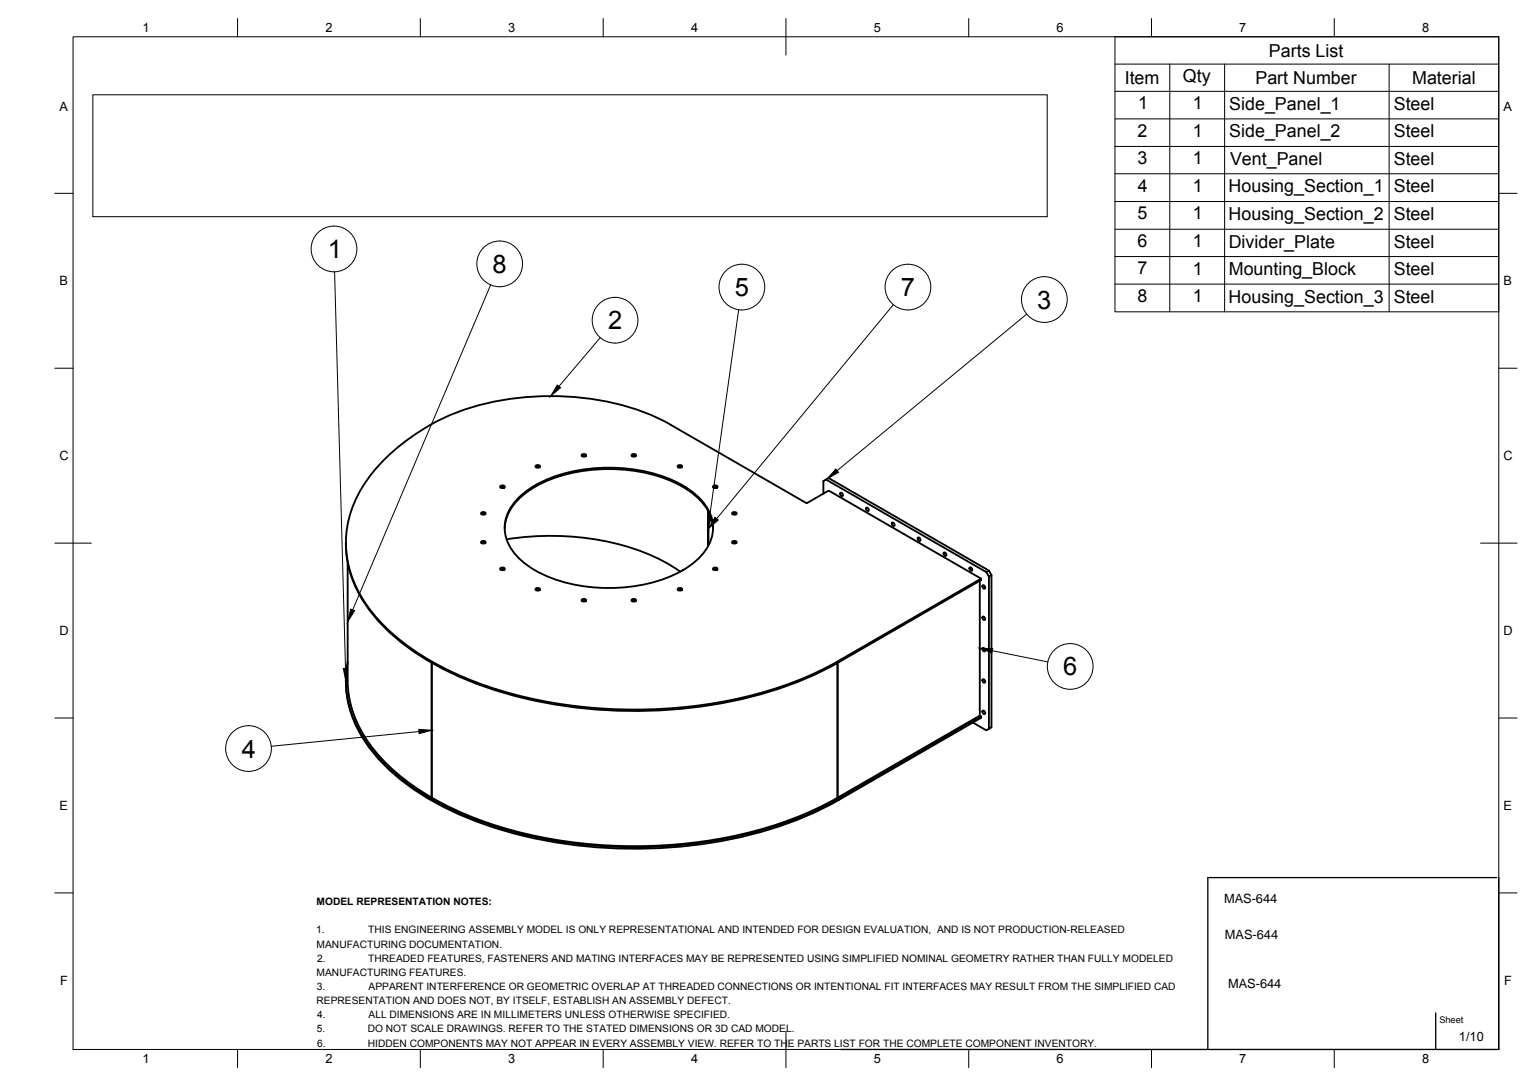
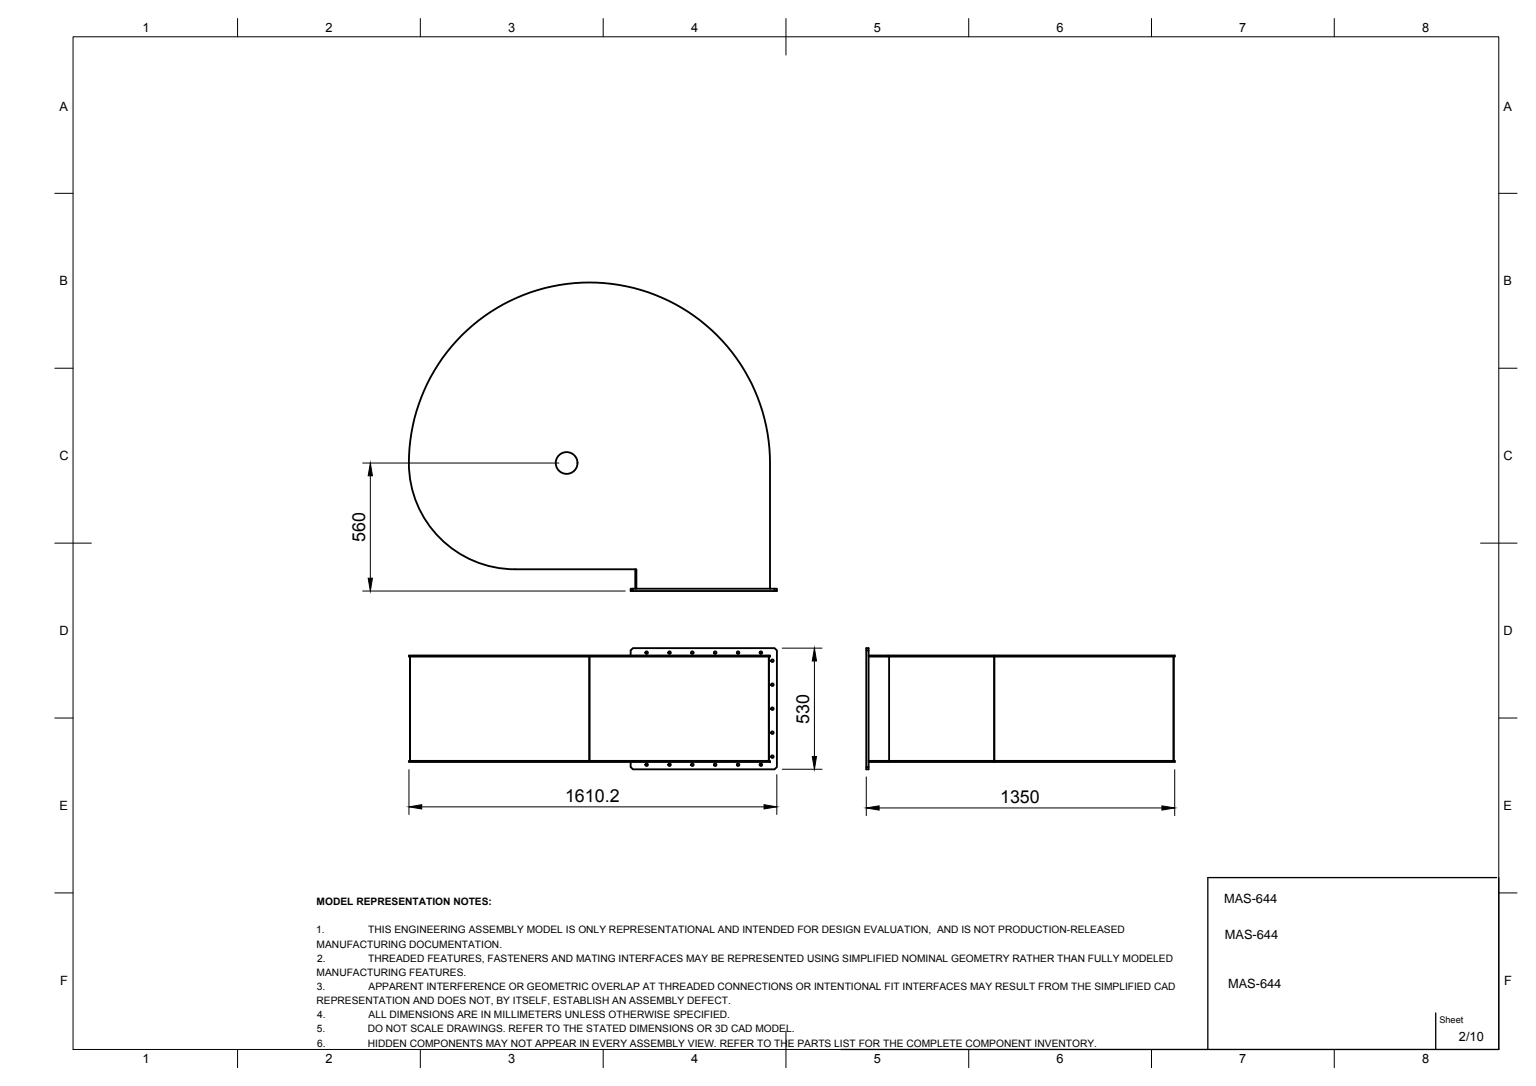
ISO-10303-21;
HEADER;
FILE_DESCRIPTION((''),'2;1');
FILE_NAME('MAS-644','2026-10-09T11:38:21-07:00',(''),(''),'','','');
FILE_SCHEMA (('AUTOMOTIVE_DESIGN { 1 0 10303 214 3 1 1 }'));
ENDSEC;
DATA;
#10 = MECHANICAL_DESIGN_GEOMETRIC_PRESENTATION_REPRESENTATION('',(#59,#60,
#61,#62,#63,#64,#65,#66),#3619) ;
#11 = ITEM_DEFINED_TRANSFORMATION($,$,#2181,#2401) ;
#12 = ITEM_DEFINED_TRANSFORMATION($,$,#2197,#2402) ;
#13 = ITEM_DEFINED_TRANSFORMATION($,$,#2261,#2403) ;
#14 = ITEM_DEFINED_TRANSFORMATION($,$,#2342,#2404) ;
#15 = ITEM_DEFINED_TRANSFORMATION($,$,#2353,#2405) ;
#16 = ITEM_DEFINED_TRANSFORMATION($,$,#2364,#2406) ;
#17 = ITEM_DEFINED_TRANSFORMATION($,$,#2371,#2407) ;
#18 = ITEM_DEFINED_TRANSFORMATION($,$,#2390,#2408) ;
#19 = (
REPRESENTATION_RELATIONSHIP($,$,#3651,#3650)
REPRESENTATION_RELATIONSHIP_WITH_TRANSFORMATION(#11)
SHAPE_REPRESENTATION_RELATIONSHIP()
) ;
#20 = (
REPRESENTATION_RELATIONSHIP($,$,#3652,#3650)
REPRESENTATION_RELATIONSHIP_WITH_TRANSFORMATION(#12)
SHAPE_REPRESENTATION_RELATIONSHIP()
) ;
#21 = (
REPRESENTATION_RELATIONSHIP($,$,#3653,#3650)
REPRESENTATION_RELATIONSHIP_WITH_TRANSFORMATION(#13)
SHAPE_REPRESENTATION_RELATIONSHIP()
) ;
#22 = (
REPRESENTATION_RELATIONSHIP($,$,#3654,#3650)
REPRESENTATION_RELATIONSHIP_WITH_TRANSFORMATION(#14)
SHAPE_REPRESENTATION_RELATIONSHIP()
) ;
#23 = (
REPRESENTATION_RELATIONSHIP($,$,#3655,#3650)
REPRESENTATION_RELATIONSHIP_WITH_TRANSFORMATION(#15)
SHAPE_REPRESENTATION_RELATIONSHIP()
) ;
#24 = (
REPRESENTATION_RELATIONSHIP($,$,#3656,#3650)
REPRESENTATION_RELATIONSHIP_WITH_TRANSFORMATION(#16)
SHAPE_REPRESENTATION_RELATIONSHIP()
) ;
#25 = (
REPRESENTATION_RELATIONSHIP($,$,#3657,#3650)
REPRESENTATION_RELATIONSHIP_WITH_TRANSFORMATION(#17)
SHAPE_REPRESENTATION_RELATIONSHIP()
) ;
#26 = (
REPRESENTATION_RELATIONSHIP($,$,#3658,#3650)
REPRESENTATION_RELATIONSHIP_WITH_TRANSFORMATION(#18)
SHAPE_REPRESENTATION_RELATIONSHIP()
) ;
#27 = CONTEXT_DEPENDENT_SHAPE_REPRESENTATION(#19,#3642) ;
#28 = CONTEXT_DEPENDENT_SHAPE_REPRESENTATION(#20,#3643) ;
#29 = CONTEXT_DEPENDENT_SHAPE_REPRESENTATION(#21,#3644) ;
#30 = CONTEXT_DEPENDENT_SHAPE_REPRESENTATION(#22,#3645) ;
#31 = CONTEXT_DEPENDENT_SHAPE_REPRESENTATION(#23,#3646) ;
#32 = CONTEXT_DEPENDENT_SHAPE_REPRESENTATION(#24,#3647) ;
#33 = CONTEXT_DEPENDENT_SHAPE_REPRESENTATION(#25,#3648) ;
#34 = CONTEXT_DEPENDENT_SHAPE_REPRESENTATION(#26,#3649) ;
#35 = NEXT_ASSEMBLY_USAGE_OCCURRENCE('Side_Panel_1:1','Side_Panel_1:1',
'Side_Panel_1:1',#3660,#3661,'Side_Panel_1:1') ;
#36 = NEXT_ASSEMBLY_USAGE_OCCURRENCE('Side_Panel_2:1','Side_Panel_2:1',
'Side_Panel_2:1',#3660,#3662,'Side_Panel_2:1') ;
#37 = NEXT_ASSEMBLY_USAGE_OCCURRENCE('Vent_Panel:1','Vent_Panel:1',
'Vent_Panel:1',#3660,#3663,'Vent_Panel:1') ;
#38 = NEXT_ASSEMBLY_USAGE_OCCURRENCE('Housing_Section_1:1',
'Housing_Section_1:1','Housing_Section_1:1',#3660,#3664,
'Housing_Section_1:1') ;
#39 = NEXT_ASSEMBLY_USAGE_OCCURRENCE('Housing_Section_2:1',
'Housing_Section_2:1','Housing_Section_2:1',#3660,#3665,
'Housing_Section_2:1') ;
#40 = NEXT_ASSEMBLY_USAGE_OCCURRENCE('Divider_Plate:1','Divider_Plate:1',
'Divider_Plate:1',#3660,#3666,'Divider_Plate:1') ;
#41 = NEXT_ASSEMBLY_USAGE_OCCURRENCE('Mounting_Block:1',
'Mounting_Block:1','Mounting_Block:1',#3660,#3667,'Mounting_Block:1') ;
#42 = NEXT_ASSEMBLY_USAGE_OCCURRENCE('Housing_Section_3:1',
'Housing_Section_3:1','Housing_Section_3:1',#3660,#3668,
'Housing_Section_3:1') ;
#43 = SHAPE_REPRESENTATION_RELATIONSHIP('SRR','None',#3651,#51) ;
#44 = SHAPE_REPRESENTATION_RELATIONSHIP('SRR','None',#3652,#52) ;
#45 = SHAPE_REPRESENTATION_RELATIONSHIP('SRR','None',#3653,#53) ;
#46 = SHAPE_REPRESENTATION_RELATIONSHIP('SRR','None',#3654,#54) ;
#47 = SHAPE_REPRESENTATION_RELATIONSHIP('SRR','None',#3655,#55) ;
#48 = SHAPE_REPRESENTATION_RELATIONSHIP('SRR','None',#3656,#56) ;
#49 = SHAPE_REPRESENTATION_RELATIONSHIP('SRR','None',#3657,#57) ;
#50 = SHAPE_REPRESENTATION_RELATIONSHIP('SRR','None',#3658,#58) ;
#51 = ADVANCED_BREP_SHAPE_REPRESENTATION('',(#67),#3611) ;
#52 = ADVANCED_BREP_SHAPE_REPRESENTATION('',(#68),#3612) ;
#53 = ADVANCED_BREP_SHAPE_REPRESENTATION('',(#69),#3613) ;
#54 = ADVANCED_BREP_SHAPE_REPRESENTATION('',(#70),#3614) ;
#55 = ADVANCED_BREP_SHAPE_REPRESENTATION('',(#71),#3615) ;
#56 = ADVANCED_BREP_SHAPE_REPRESENTATION('',(#72),#3616) ;
#57 = ADVANCED_BREP_SHAPE_REPRESENTATION('',(#73),#3617) ;
#58 = ADVANCED_BREP_SHAPE_REPRESENTATION('',(#74),#3618) ;
#59 = STYLED_ITEM('',(#3700),#67) ;
#60 = STYLED_ITEM('',(#3700),#68) ;
#61 = STYLED_ITEM('',(#3700),#69) ;
#62 = STYLED_ITEM('',(#3700),#70) ;
#63 = STYLED_ITEM('',(#3700),#71) ;
#64 = STYLED_ITEM('',(#3700),#72) ;
#65 = STYLED_ITEM('',(#3700),#73) ;
#66 = STYLED_ITEM('',(#3700),#74) ;
#67 = MANIFOLD_SOLID_BREP('Body1',#2083) ;
#68 = MANIFOLD_SOLID_BREP('Body1',#2084) ;
#69 = MANIFOLD_SOLID_BREP('Body1',#2085) ;
#70 = MANIFOLD_SOLID_BREP('Body1',#2086) ;
#71 = MANIFOLD_SOLID_BREP('Body1',#2087) ;
#72 = MANIFOLD_SOLID_BREP('Body1',#2088) ;
#73 = MANIFOLD_SOLID_BREP('Body1',#2089) ;
#74 = MANIFOLD_SOLID_BREP('Body1',#2090) ;
#75 = FACE_BOUND('',#329,.T.) ;
#76 = FACE_BOUND('',#331,.T.) ;
#77 = FACE_BOUND('',#356,.T.) ;
#78 = FACE_BOUND('',#357,.T.) ;
#79 = FACE_BOUND('',#358,.T.) ;
#80 = FACE_BOUND('',#359,.T.) ;
#81 = FACE_BOUND('',#360,.T.) ;
#82 = FACE_BOUND('',#361,.T.) ;
#83 = FACE_BOUND('',#362,.T.) ;
#84 = FACE_BOUND('',#363,.T.) ;
#85 = FACE_BOUND('',#364,.T.) ;
#86 = FACE_BOUND('',#365,.T.) ;
#87 = FACE_BOUND('',#366,.T.) ;
#88 = FACE_BOUND('',#367,.T.) ;
#89 = FACE_BOUND('',#368,.T.) ;
#90 = FACE_BOUND('',#369,.T.) ;
#91 = FACE_BOUND('',#370,.T.) ;
#92 = FACE_BOUND('',#371,.T.) ;
#93 = FACE_BOUND('',#372,.T.) ;
#94 = FACE_BOUND('',#374,.T.) ;
#95 = FACE_BOUND('',#375,.T.) ;
#96 = FACE_BOUND('',#376,.T.) ;
#97 = FACE_BOUND('',#377,.T.) ;
#98 = FACE_BOUND('',#378,.T.) ;
#99 = FACE_BOUND('',#379,.T.) ;
#100 = FACE_BOUND('',#380,.T.) ;
#101 = FACE_BOUND('',#381,.T.) ;
#102 = FACE_BOUND('',#382,.T.) ;
#103 = FACE_BOUND('',#383,.T.) ;
#104 = FACE_BOUND('',#384,.T.) ;
#105 = FACE_BOUND('',#385,.T.) ;
#106 = FACE_BOUND('',#386,.T.) ;
#107 = FACE_BOUND('',#387,.T.) ;
#108 = FACE_BOUND('',#388,.T.) ;
#109 = FACE_BOUND('',#389,.T.) ;
#110 = FACE_BOUND('',#390,.T.) ;
#111 = FACE_BOUND('',#414,.T.) ;
#112 = FACE_BOUND('',#415,.T.) ;
#113 = FACE_BOUND('',#416,.T.) ;
#114 = FACE_BOUND('',#417,.T.) ;
#115 = FACE_BOUND('',#418,.T.) ;
#116 = FACE_BOUND('',#419,.T.) ;
#117 = FACE_BOUND('',#420,.T.) ;
#118 = FACE_BOUND('',#421,.T.) ;
#119 = FACE_BOUND('',#422,.T.) ;
#120 = FACE_BOUND('',#423,.T.) ;
#121 = FACE_BOUND('',#424,.T.) ;
#122 = FACE_BOUND('',#425,.T.) ;
#123 = FACE_BOUND('',#426,.T.) ;
#124 = FACE_BOUND('',#427,.T.) ;
#125 = FACE_BOUND('',#428,.T.) ;
#126 = FACE_BOUND('',#429,.T.) ;
#127 = FACE_BOUND('',#430,.T.) ;
#128 = FACE_BOUND('',#431,.T.) ;
#129 = FACE_BOUND('',#432,.T.) ;
#130 = FACE_BOUND('',#433,.T.) ;
#131 = FACE_BOUND('',#434,.T.) ;
#132 = FACE_BOUND('',#435,.T.) ;
#133 = FACE_BOUND('',#436,.T.) ;
#134 = FACE_BOUND('',#438,.T.) ;
#135 = FACE_BOUND('',#439,.T.) ;
#136 = FACE_BOUND('',#440,.T.) ;
#137 = FACE_BOUND('',#441,.T.) ;
#138 = FACE_BOUND('',#442,.T.) ;
#139 = FACE_BOUND('',#443,.T.) ;
#140 = FACE_BOUND('',#444,.T.) ;
#141 = FACE_BOUND('',#445,.T.) ;
#142 = FACE_BOUND('',#446,.T.) ;
#143 = FACE_BOUND('',#447,.T.) ;
#144 = FACE_BOUND('',#448,.T.) ;
#145 = FACE_BOUND('',#449,.T.) ;
#146 = FACE_BOUND('',#450,.T.) ;
#147 = FACE_BOUND('',#451,.T.) ;
#148 = FACE_BOUND('',#452,.T.) ;
#149 = FACE_BOUND('',#453,.T.) ;
#150 = FACE_BOUND('',#454,.T.) ;
#151 = FACE_BOUND('',#455,.T.) ;
#152 = FACE_BOUND('',#456,.T.) ;
#153 = FACE_BOUND('',#457,.T.) ;
#154 = FACE_BOUND('',#458,.T.) ;
#155 = FACE_BOUND('',#459,.T.) ;
#156 = FACE_BOUND('',#460,.T.) ;
#157 = PLANE('',#2185) ;
#158 = PLANE('',#2186) ;
#159 = PLANE('',#2187) ;
#160 = PLANE('',#2188) ;
#161 = PLANE('',#2195) ;
#162 = PLANE('',#2196) ;
#163 = PLANE('',#2249) ;
#164 = PLANE('',#2250) ;
#165 = PLANE('',#2251) ;
#166 = PLANE('',#2252) ;
#167 = PLANE('',#2259) ;
#168 = PLANE('',#2260) ;
#169 = PLANE('',#2328) ;
#170 = PLANE('',#2329) ;
#171 = PLANE('',#2330) ;
#172 = PLANE('',#2331) ;
#173 = PLANE('',#2332) ;
#174 = PLANE('',#2333) ;
#175 = PLANE('',#2334) ;
#176 = PLANE('',#2335) ;
#177 = PLANE('',#2336) ;
#178 = PLANE('',#2337) ;
#179 = PLANE('',#2338) ;
#180 = PLANE('',#2339) ;
#181 = PLANE('',#2340) ;
#182 = PLANE('',#2341) ;
#183 = PLANE('',#2346) ;
#184 = PLANE('',#2350) ;
#185 = PLANE('',#2351) ;
#186 = PLANE('',#2352) ;
#187 = PLANE('',#2354) ;
#188 = PLANE('',#2358) ;
#189 = PLANE('',#2362) ;
#190 = PLANE('',#2363) ;
#191 = PLANE('',#2365) ;
#192 = PLANE('',#2366) ;
#193 = PLANE('',#2367) ;
#194 = PLANE('',#2368) ;
#195 = PLANE('',#2369) ;
#196 = PLANE('',#2370) ;
#197 = PLANE('',#2372) ;
#198 = PLANE('',#2375) ;
#199 = PLANE('',#2376) ;
#200 = PLANE('',#2379) ;
#201 = PLANE('',#2380) ;
#202 = PLANE('',#2381) ;
#203 = PLANE('',#2382) ;
#204 = PLANE('',#2384) ;
#205 = PLANE('',#2385) ;
#206 = PLANE('',#2386) ;
#207 = PLANE('',#2388) ;
#208 = PLANE('',#2389) ;
#209 = PLANE('',#2394) ;
#210 = PLANE('',#2398) ;
#211 = PLANE('',#2399) ;
#212 = PLANE('',#2400) ;
#213 = FACE_OUTER_BOUND('',#321,.T.) ;
#214 = FACE_OUTER_BOUND('',#322,.T.) ;
#215 = FACE_OUTER_BOUND('',#323,.T.) ;
#216 = FACE_OUTER_BOUND('',#324,.T.) ;
#217 = FACE_OUTER_BOUND('',#325,.T.) ;
#218 = FACE_OUTER_BOUND('',#326,.T.) ;
#219 = FACE_OUTER_BOUND('',#327,.T.) ;
#220 = FACE_OUTER_BOUND('',#328,.T.) ;
#221 = FACE_OUTER_BOUND('',#330,.T.) ;
#222 = FACE_OUTER_BOUND('',#332,.T.) ;
#223 = FACE_OUTER_BOUND('',#333,.T.) ;
#224 = FACE_OUTER_BOUND('',#334,.T.) ;
#225 = FACE_OUTER_BOUND('',#335,.T.) ;
#226 = FACE_OUTER_BOUND('',#336,.T.) ;
#227 = FACE_OUTER_BOUND('',#337,.T.) ;
#228 = FACE_OUTER_BOUND('',#338,.T.) ;
#229 = FACE_OUTER_BOUND('',#339,.T.) ;
#230 = FACE_OUTER_BOUND('',#340,.T.) ;
#231 = FACE_OUTER_BOUND('',#341,.T.) ;
#232 = FACE_OUTER_BOUND('',#342,.T.) ;
#233 = FACE_OUTER_BOUND('',#343,.T.) ;
#234 = FACE_OUTER_BOUND('',#344,.T.) ;
#235 = FACE_OUTER_BOUND('',#345,.T.) ;
#236 = FACE_OUTER_BOUND('',#346,.T.) ;
#237 = FACE_OUTER_BOUND('',#347,.T.) ;
#238 = FACE_OUTER_BOUND('',#348,.T.) ;
#239 = FACE_OUTER_BOUND('',#349,.T.) ;
#240 = FACE_OUTER_BOUND('',#350,.T.) ;
#241 = FACE_OUTER_BOUND('',#351,.T.) ;
#242 = FACE_OUTER_BOUND('',#352,.T.) ;
#243 = FACE_OUTER_BOUND('',#353,.T.) ;
#244 = FACE_OUTER_BOUND('',#354,.T.) ;
#245 = FACE_OUTER_BOUND('',#355,.T.) ;
#246 = FACE_OUTER_BOUND('',#373,.T.) ;
#247 = FACE_OUTER_BOUND('',#391,.T.) ;
#248 = FACE_OUTER_BOUND('',#392,.T.) ;
#249 = FACE_OUTER_BOUND('',#393,.T.) ;
#250 = FACE_OUTER_BOUND('',#394,.T.) ;
#251 = FACE_OUTER_BOUND('',#395,.T.) ;
#252 = FACE_OUTER_BOUND('',#396,.T.) ;
#253 = FACE_OUTER_BOUND('',#397,.T.) ;
#254 = FACE_OUTER_BOUND('',#398,.T.) ;
#255 = FACE_OUTER_BOUND('',#399,.T.) ;
#256 = FACE_OUTER_BOUND('',#400,.T.) ;
#257 = FACE_OUTER_BOUND('',#401,.T.) ;
#258 = FACE_OUTER_BOUND('',#402,.T.) ;
#259 = FACE_OUTER_BOUND('',#403,.T.) ;
#260 = FACE_OUTER_BOUND('',#404,.T.) ;
#261 = FACE_OUTER_BOUND('',#405,.T.) ;
#262 = FACE_OUTER_BOUND('',#406,.T.) ;
#263 = FACE_OUTER_BOUND('',#407,.T.) ;
#264 = FACE_OUTER_BOUND('',#408,.T.) ;
#265 = FACE_OUTER_BOUND('',#409,.T.) ;
#266 = FACE_OUTER_BOUND('',#410,.T.) ;
#267 = FACE_OUTER_BOUND('',#411,.T.) ;
#268 = FACE_OUTER_BOUND('',#412,.T.) ;
#269 = FACE_OUTER_BOUND('',#413,.T.) ;
#270 = FACE_OUTER_BOUND('',#437,.T.) ;
#271 = FACE_OUTER_BOUND('',#461,.T.) ;
#272 = FACE_OUTER_BOUND('',#462,.T.) ;
#273 = FACE_OUTER_BOUND('',#463,.T.) ;
#274 = FACE_OUTER_BOUND('',#464,.T.) ;
#275 = FACE_OUTER_BOUND('',#465,.T.) ;
#276 = FACE_OUTER_BOUND('',#466,.T.) ;
#277 = FACE_OUTER_BOUND('',#467,.T.) ;
#278 = FACE_OUTER_BOUND('',#468,.T.) ;
#279 = FACE_OUTER_BOUND('',#469,.T.) ;
#280 = FACE_OUTER_BOUND('',#470,.T.) ;
#281 = FACE_OUTER_BOUND('',#471,.T.) ;
#282 = FACE_OUTER_BOUND('',#472,.T.) ;
#283 = FACE_OUTER_BOUND('',#473,.T.) ;
#284 = FACE_OUTER_BOUND('',#474,.T.) ;
#285 = FACE_OUTER_BOUND('',#475,.T.) ;
#286 = FACE_OUTER_BOUND('',#476,.T.) ;
#287 = FACE_OUTER_BOUND('',#477,.T.) ;
#288 = FACE_OUTER_BOUND('',#478,.T.) ;
#289 = FACE_OUTER_BOUND('',#479,.T.) ;
#290 = FACE_OUTER_BOUND('',#480,.T.) ;
#291 = FACE_OUTER_BOUND('',#481,.T.) ;
#292 = FACE_OUTER_BOUND('',#482,.T.) ;
#293 = FACE_OUTER_BOUND('',#483,.T.) ;
#294 = FACE_OUTER_BOUND('',#484,.T.) ;
#295 = FACE_OUTER_BOUND('',#485,.T.) ;
#296 = FACE_OUTER_BOUND('',#486,.T.) ;
#297 = FACE_OUTER_BOUND('',#487,.T.) ;
#298 = FACE_OUTER_BOUND('',#488,.T.) ;
#299 = FACE_OUTER_BOUND('',#489,.T.) ;
#300 = FACE_OUTER_BOUND('',#490,.T.) ;
#301 = FACE_OUTER_BOUND('',#491,.T.) ;
#302 = FACE_OUTER_BOUND('',#492,.T.) ;
#303 = FACE_OUTER_BOUND('',#493,.T.) ;
#304 = FACE_OUTER_BOUND('',#494,.T.) ;
#305 = FACE_OUTER_BOUND('',#495,.T.) ;
#306 = FACE_OUTER_BOUND('',#496,.T.) ;
#307 = FACE_OUTER_BOUND('',#497,.T.) ;
#308 = FACE_OUTER_BOUND('',#498,.T.) ;
#309 = FACE_OUTER_BOUND('',#499,.T.) ;
#310 = FACE_OUTER_BOUND('',#500,.T.) ;
#311 = FACE_OUTER_BOUND('',#501,.T.) ;
#312 = FACE_OUTER_BOUND('',#502,.T.) ;
#313 = FACE_OUTER_BOUND('',#503,.T.) ;
#314 = FACE_OUTER_BOUND('',#504,.T.) ;
#315 = FACE_OUTER_BOUND('',#505,.T.) ;
#316 = FACE_OUTER_BOUND('',#506,.T.) ;
#317 = FACE_OUTER_BOUND('',#507,.T.) ;
#318 = FACE_OUTER_BOUND('',#508,.T.) ;
#319 = FACE_OUTER_BOUND('',#509,.T.) ;
#320 = FACE_OUTER_BOUND('',#510,.T.) ;
#321 = EDGE_LOOP('',(#1387,#1388,#1389,#1390)) ;
#322 = EDGE_LOOP('',(#1391,#1392,#1393,#1394)) ;
#323 = EDGE_LOOP('',(#1395,#1396,#1397,#1398)) ;
#324 = EDGE_LOOP('',(#1399,#1400,#1401,#1402)) ;
#325 = EDGE_LOOP('',(#1403,#1404,#1405,#1406)) ;
#326 = EDGE_LOOP('',(#1407,#1408,#1409,#1410)) ;
#327 = EDGE_LOOP('',(#1411,#1412,#1413,#1414)) ;
#328 = EDGE_LOOP('',(#1415,#1416,#1417,#1418,#1419,#1420)) ;
#329 = EDGE_LOOP('',(#1421)) ;
#330 = EDGE_LOOP('',(#1422,#1423,#1424,#1425,#1426,#1427)) ;
#331 = EDGE_LOOP('',(#1428)) ;
#332 = EDGE_LOOP('',(#1429,#1430,#1431,#1432)) ;
#333 = EDGE_LOOP('',(#1433,#1434,#1435,#1436)) ;
#334 = EDGE_LOOP('',(#1437,#1438,#1439,#1440)) ;
#335 = EDGE_LOOP('',(#1441,#1442,#1443,#1444)) ;
#336 = EDGE_LOOP('',(#1445,#1446,#1447,#1448)) ;
#337 = EDGE_LOOP('',(#1449,#1450,#1451,#1452)) ;
#338 = EDGE_LOOP('',(#1453,#1454,#1455,#1456)) ;
#339 = EDGE_LOOP('',(#1457,#1458,#1459,#1460)) ;
#340 = EDGE_LOOP('',(#1461,#1462,#1463,#1464)) ;
#341 = EDGE_LOOP('',(#1465,#1466,#1467,#1468)) ;
#342 = EDGE_LOOP('',(#1469,#1470,#1471,#1472)) ;
#343 = EDGE_LOOP('',(#1473,#1474,#1475,#1476)) ;
#344 = EDGE_LOOP('',(#1477,#1478,#1479,#1480)) ;
#345 = EDGE_LOOP('',(#1481,#1482,#1483,#1484)) ;
#346 = EDGE_LOOP('',(#1485,#1486,#1487,#1488)) ;
#347 = EDGE_LOOP('',(#1489,#1490,#1491,#1492)) ;
#348 = EDGE_LOOP('',(#1493,#1494,#1495,#1496)) ;
#349 = EDGE_LOOP('',(#1497,#1498,#1499,#1500)) ;
#350 = EDGE_LOOP('',(#1501,#1502,#1503,#1504)) ;
#351 = EDGE_LOOP('',(#1505,#1506,#1507,#1508)) ;
#352 = EDGE_LOOP('',(#1509,#1510,#1511,#1512)) ;
#353 = EDGE_LOOP('',(#1513,#1514,#1515,#1516)) ;
#354 = EDGE_LOOP('',(#1517,#1518,#1519,#1520)) ;
#355 = EDGE_LOOP('',(#1521,#1522,#1523,#1524,#1525,#1526)) ;
#356 = EDGE_LOOP('',(#1527)) ;
#357 = EDGE_LOOP('',(#1528)) ;
#358 = EDGE_LOOP('',(#1529)) ;
#359 = EDGE_LOOP('',(#1530)) ;
#360 = EDGE_LOOP('',(#1531)) ;
#361 = EDGE_LOOP('',(#1532)) ;
#362 = EDGE_LOOP('',(#1533)) ;
#363 = EDGE_LOOP('',(#1534)) ;
#364 = EDGE_LOOP('',(#1535)) ;
#365 = EDGE_LOOP('',(#1536)) ;
#366 = EDGE_LOOP('',(#1537)) ;
#367 = EDGE_LOOP('',(#1538)) ;
#368 = EDGE_LOOP('',(#1539)) ;
#369 = EDGE_LOOP('',(#1540)) ;
#370 = EDGE_LOOP('',(#1541)) ;
#371 = EDGE_LOOP('',(#1542)) ;
#372 = EDGE_LOOP('',(#1543)) ;
#373 = EDGE_LOOP('',(#1544,#1545,#1546,#1547,#1548,#1549)) ;
#374 = EDGE_LOOP('',(#1550)) ;
#375 = EDGE_LOOP('',(#1551)) ;
#376 = EDGE_LOOP('',(#1552)) ;
#377 = EDGE_LOOP('',(#1553)) ;
#378 = EDGE_LOOP('',(#1554)) ;
#379 = EDGE_LOOP('',(#1555)) ;
#380 = EDGE_LOOP('',(#1556)) ;
#381 = EDGE_LOOP('',(#1557)) ;
#382 = EDGE_LOOP('',(#1558)) ;
#383 = EDGE_LOOP('',(#1559)) ;
#384 = EDGE_LOOP('',(#1560)) ;
#385 = EDGE_LOOP('',(#1561)) ;
#386 = EDGE_LOOP('',(#1562)) ;
#387 = EDGE_LOOP('',(#1563)) ;
#388 = EDGE_LOOP('',(#1564)) ;
#389 = EDGE_LOOP('',(#1565)) ;
#390 = EDGE_LOOP('',(#1566)) ;
#391 = EDGE_LOOP('',(#1567,#1568,#1569,#1570)) ;
#392 = EDGE_LOOP('',(#1571,#1572,#1573,#1574)) ;
#393 = EDGE_LOOP('',(#1575,#1576,#1577,#1578)) ;
#394 = EDGE_LOOP('',(#1579,#1580,#1581,#1582)) ;
#395 = EDGE_LOOP('',(#1583,#1584,#1585,#1586)) ;
#396 = EDGE_LOOP('',(#1587,#1588,#1589,#1590)) ;
#397 = EDGE_LOOP('',(#1591,#1592,#1593,#1594)) ;
#398 = EDGE_LOOP('',(#1595,#1596,#1597,#1598)) ;
#399 = EDGE_LOOP('',(#1599,#1600,#1601,#1602)) ;
#400 = EDGE_LOOP('',(#1603,#1604,#1605,#1606)) ;
#401 = EDGE_LOOP('',(#1607,#1608,#1609,#1610)) ;
#402 = EDGE_LOOP('',(#1611,#1612,#1613,#1614)) ;
#403 = EDGE_LOOP('',(#1615,#1616,#1617,#1618)) ;
#404 = EDGE_LOOP('',(#1619,#1620,#1621,#1622)) ;
#405 = EDGE_LOOP('',(#1623,#1624,#1625,#1626)) ;
#406 = EDGE_LOOP('',(#1627,#1628,#1629,#1630)) ;
#407 = EDGE_LOOP('',(#1631,#1632,#1633,#1634)) ;
#408 = EDGE_LOOP('',(#1635,#1636,#1637,#1638)) ;
#409 = EDGE_LOOP('',(#1639,#1640,#1641,#1642)) ;
#410 = EDGE_LOOP('',(#1643,#1644,#1645,#1646)) ;
#411 = EDGE_LOOP('',(#1647,#1648,#1649,#1650)) ;
#412 = EDGE_LOOP('',(#1651,#1652,#1653,#1654)) ;
#413 = EDGE_LOOP('',(#1655,#1656,#1657,#1658,#1659,#1660,#1661,#1662)) ;
#414 = EDGE_LOOP('',(#1663,#1664,#1665,#1666)) ;
#415 = EDGE_LOOP('',(#1667)) ;
#416 = EDGE_LOOP('',(#1668)) ;
#417 = EDGE_LOOP('',(#1669)) ;
#418 = EDGE_LOOP('',(#1670)) ;
#419 = EDGE_LOOP('',(#1671)) ;
#420 = EDGE_LOOP('',(#1672)) ;
#421 = EDGE_LOOP('',(#1673)) ;
#422 = EDGE_LOOP('',(#1674)) ;
#423 = EDGE_LOOP('',(#1675)) ;
#424 = EDGE_LOOP('',(#1676)) ;
#425 = EDGE_LOOP('',(#1677)) ;
#426 = EDGE_LOOP('',(#1678)) ;
#427 = EDGE_LOOP('',(#1679)) ;
#428 = EDGE_LOOP('',(#1680)) ;
#429 = EDGE_LOOP('',(#1681)) ;
#430 = EDGE_LOOP('',(#1682)) ;
#431 = EDGE_LOOP('',(#1683)) ;
#432 = EDGE_LOOP('',(#1684)) ;
#433 = EDGE_LOOP('',(#1685)) ;
#434 = EDGE_LOOP('',(#1686)) ;
#435 = EDGE_LOOP('',(#1687)) ;
#436 = EDGE_LOOP('',(#1688)) ;
#437 = EDGE_LOOP('',(#1689,#1690,#1691,#1692,#1693,#1694,#1695,#1696)) ;
#438 = EDGE_LOOP('',(#1697,#1698,#1699,#1700)) ;
#439 = EDGE_LOOP('',(#1701)) ;
#440 = EDGE_LOOP('',(#1702)) ;
#441 = EDGE_LOOP('',(#1703)) ;
#442 = EDGE_LOOP('',(#1704)) ;
#443 = EDGE_LOOP('',(#1705)) ;
#444 = EDGE_LOOP('',(#1706)) ;
#445 = EDGE_LOOP('',(#1707)) ;
#446 = EDGE_LOOP('',(#1708)) ;
#447 = EDGE_LOOP('',(#1709)) ;
#448 = EDGE_LOOP('',(#1710)) ;
#449 = EDGE_LOOP('',(#1711)) ;
#450 = EDGE_LOOP('',(#1712)) ;
#451 = EDGE_LOOP('',(#1713)) ;
#452 = EDGE_LOOP('',(#1714)) ;
#453 = EDGE_LOOP('',(#1715)) ;
#454 = EDGE_LOOP('',(#1716)) ;
#455 = EDGE_LOOP('',(#1717)) ;
#456 = EDGE_LOOP('',(#1718)) ;
#457 = EDGE_LOOP('',(#1719)) ;
#458 = EDGE_LOOP('',(#1720)) ;
#459 = EDGE_LOOP('',(#1721)) ;
#460 = EDGE_LOOP('',(#1722)) ;
#461 = EDGE_LOOP('',(#1723,#1724,#1725,#1726)) ;
#462 = EDGE_LOOP('',(#1727,#1728,#1729,#1730)) ;
#463 = EDGE_LOOP('',(#1731,#1732,#1733,#1734)) ;
#464 = EDGE_LOOP('',(#1735,#1736,#1737,#1738)) ;
#465 = EDGE_LOOP('',(#1739,#1740,#1741,#1742)) ;
#466 = EDGE_LOOP('',(#1743,#1744,#1745,#1746)) ;
#467 = EDGE_LOOP('',(#1747,#1748,#1749,#1750)) ;
#468 = EDGE_LOOP('',(#1751,#1752,#1753,#1754)) ;
#469 = EDGE_LOOP('',(#1755,#1756,#1757,#1758)) ;
#470 = EDGE_LOOP('',(#1759,#1760,#1761,#1762)) ;
#471 = EDGE_LOOP('',(#1763,#1764,#1765,#1766)) ;
#472 = EDGE_LOOP('',(#1767,#1768,#1769,#1770)) ;
#473 = EDGE_LOOP('',(#1771,#1772,#1773,#1774)) ;
#474 = EDGE_LOOP('',(#1775,#1776,#1777,#1778)) ;
#475 = EDGE_LOOP('',(#1779,#1780,#1781,#1782)) ;
#476 = EDGE_LOOP('',(#1783,#1784,#1785,#1786)) ;
#477 = EDGE_LOOP('',(#1787,#1788,#1789,#1790)) ;
#478 = EDGE_LOOP('',(#1791,#1792,#1793,#1794)) ;
#479 = EDGE_LOOP('',(#1795,#1796,#1797,#1798)) ;
#480 = EDGE_LOOP('',(#1799,#1800,#1801,#1802)) ;
#481 = EDGE_LOOP('',(#1803,#1804,#1805,#1806)) ;
#482 = EDGE_LOOP('',(#1807,#1808,#1809,#1810)) ;
#483 = EDGE_LOOP('',(#1811,#1812,#1813,#1814)) ;
#484 = EDGE_LOOP('',(#1815,#1816,#1817,#1818)) ;
#485 = EDGE_LOOP('',(#1819,#1820,#1821,#1822)) ;
#486 = EDGE_LOOP('',(#1823,#1824,#1825,#1826)) ;
#487 = EDGE_LOOP('',(#1827,#1828,#1829,#1830)) ;
#488 = EDGE_LOOP('',(#1831,#1832,#1833,#1834)) ;
#489 = EDGE_LOOP('',(#1835,#1836,#1837,#1838)) ;
#490 = EDGE_LOOP('',(#1839,#1840,#1841,#1842)) ;
#491 = EDGE_LOOP('',(#1843,#1844,#1845,#1846)) ;
#492 = EDGE_LOOP('',(#1847,#1848,#1849,#1850)) ;
#493 = EDGE_LOOP('',(#1851,#1852,#1853,#1854)) ;
#494 = EDGE_LOOP('',(#1855,#1856,#1857,#1858)) ;
#495 = EDGE_LOOP('',(#1859,#1860,#1861,#1862)) ;
#496 = EDGE_LOOP('',(#1863,#1864,#1865,#1866)) ;
#497 = EDGE_LOOP('',(#1867,#1868,#1869,#1870)) ;
#498 = EDGE_LOOP('',(#1871,#1872,#1873,#1874)) ;
#499 = EDGE_LOOP('',(#1875,#1876,#1877,#1878)) ;
#500 = EDGE_LOOP('',(#1879,#1880,#1881,#1882)) ;
#501 = EDGE_LOOP('',(#1883,#1884,#1885,#1886)) ;
#502 = EDGE_LOOP('',(#1887,#1888,#1889,#1890)) ;
#503 = EDGE_LOOP('',(#1891,#1892,#1893,#1894)) ;
#504 = EDGE_LOOP('',(#1895,#1896,#1897,#1898)) ;
#505 = EDGE_LOOP('',(#1899,#1900,#1901,#1902)) ;
#506 = EDGE_LOOP('',(#1903,#1904,#1905,#1906)) ;
#507 = EDGE_LOOP('',(#1907,#1908,#1909,#1910)) ;
#508 = EDGE_LOOP('',(#1911,#1912,#1913,#1914)) ;
#509 = EDGE_LOOP('',(#1915,#1916,#1917,#1918)) ;
#510 = EDGE_LOOP('',(#1919,#1920,#1921,#1922)) ;
#511 = LINE('',#3037,#675) ;
#512 = LINE('',#3042,#676) ;
#513 = LINE('',#3044,#677) ;
#514 = LINE('',#3046,#678) ;
#515 = LINE('',#3047,#679) ;
#516 = LINE('',#3050,#680) ;
#517 = LINE('',#3052,#681) ;
#518 = LINE('',#3053,#682) ;
#519 = LINE('',#3056,#683) ;
#520 = LINE('',#3058,#684) ;
#521 = LINE('',#3059,#685) ;
#522 = LINE('',#3062,#686) ;
#523 = LINE('',#3064,#687) ;
#524 = LINE('',#3065,#688) ;
#525 = LINE('',#3070,#689) ;
#526 = LINE('',#3082,#690) ;
#527 = LINE('',#3088,#691) ;
#528 = LINE('',#3094,#692) ;
#529 = LINE('',#3100,#693) ;
#530 = LINE('',#3106,#694) ;
#531 = LINE('',#3112,#695) ;
#532 = LINE('',#3118,#696) ;
#533 = LINE('',#3124,#697) ;
#534 = LINE('',#3130,#698) ;
#535 = LINE('',#3136,#699) ;
#536 = LINE('',#3142,#700) ;
#537 = LINE('',#3148,#701) ;
#538 = LINE('',#3154,#702) ;
#539 = LINE('',#3160,#703) ;
#540 = LINE('',#3166,#704) ;
#541 = LINE('',#3172,#705) ;
#542 = LINE('',#3178,#706) ;
#543 = LINE('',#3183,#707) ;
#544 = LINE('',#3185,#708) ;
#545 = LINE('',#3187,#709) ;
#546 = LINE('',#3188,#710) ;
#547 = LINE('',#3191,#711) ;
#548 = LINE('',#3193,#712) ;
#549 = LINE('',#3194,#713) ;
#550 = LINE('',#3197,#714) ;
#551 = LINE('',#3199,#715) ;
#552 = LINE('',#3200,#716) ;
#553 = LINE('',#3203,#717) ;
#554 = LINE('',#3205,#718) ;
#555 = LINE('',#3206,#719) ;
#556 = LINE('',#3211,#720) ;
#557 = LINE('',#3223,#721) ;
#558 = LINE('',#3229,#722) ;
#559 = LINE('',#3235,#723) ;
#560 = LINE('',#3241,#724) ;
#561 = LINE('',#3247,#725) ;
#562 = LINE('',#3253,#726) ;
#563 = LINE('',#3259,#727) ;
#564 = LINE('',#3265,#728) ;
#565 = LINE('',#3271,#729) ;
#566 = LINE('',#3277,#730) ;
#567 = LINE('',#3283,#731) ;
#568 = LINE('',#3289,#732) ;
#569 = LINE('',#3295,#733) ;
#570 = LINE('',#3301,#734) ;
#571 = LINE('',#3307,#735) ;
#572 = LINE('',#3313,#736) ;
#573 = LINE('',#3319,#737) ;
#574 = LINE('',#3325,#738) ;
#575 = LINE('',#3331,#739) ;
#576 = LINE('',#3337,#740) ;
#577 = LINE('',#3343,#741) ;
#578 = LINE('',#3349,#742) ;
#579 = LINE('',#3354,#743) ;
#580 = LINE('',#3356,#744) ;
#581 = LINE('',#3358,#745) ;
#582 = LINE('',#3360,#746) ;
#583 = LINE('',#3362,#747) ;
#584 = LINE('',#3364,#748) ;
#585 = LINE('',#3366,#749) ;
#586 = LINE('',#3367,#750) ;
#587 = LINE('',#3370,#751) ;
#588 = LINE('',#3372,#752) ;
#589 = LINE('',#3374,#753) ;
#590 = LINE('',#3375,#754) ;
#591 = LINE('',#3379,#755) ;
#592 = LINE('',#3381,#756) ;
#593 = LINE('',#3383,#757) ;
#594 = LINE('',#3385,#758) ;
#595 = LINE('',#3387,#759) ;
#596 = LINE('',#3389,#760) ;
#597 = LINE('',#3391,#761) ;
#598 = LINE('',#3392,#762) ;
#599 = LINE('',#3395,#763) ;
#600 = LINE('',#3397,#764) ;
#601 = LINE('',#3399,#765) ;
#602 = LINE('',#3400,#766) ;
#603 = LINE('',#3402,#767) ;
#604 = LINE('',#3403,#768) ;
#605 = LINE('',#3405,#769) ;
#606 = LINE('',#3407,#770) ;
#607 = LINE('',#3409,#771) ;
#608 = LINE('',#3411,#772) ;
#609 = LINE('',#3413,#773) ;
#610 = LINE('',#3415,#774) ;
#611 = LINE('',#3418,#775) ;
#612 = LINE('',#3419,#776) ;
#613 = LINE('',#3421,#777) ;
#614 = LINE('',#3423,#778) ;
#615 = LINE('',#3431,#779) ;
#616 = LINE('',#3434,#780) ;
#617 = LINE('',#3437,#781) ;
#618 = LINE('',#3439,#782) ;
#619 = LINE('',#3440,#783) ;
#620 = LINE('',#3445,#784) ;
#621 = LINE('',#3448,#785) ;
#622 = LINE('',#3449,#786) ;
#623 = LINE('',#3456,#787) ;
#624 = LINE('',#3458,#788) ;
#625 = LINE('',#3460,#789) ;
#626 = LINE('',#3461,#790) ;
#627 = LINE('',#3466,#791) ;
#628 = LINE('',#3470,#792) ;
#629 = LINE('',#3472,#793) ;
#630 = LINE('',#3473,#794) ;
#631 = LINE('',#3483,#795) ;
#632 = LINE('',#3485,#796) ;
#633 = LINE('',#3487,#797) ;
#634 = LINE('',#3488,#798) ;
#635 = LINE('',#3491,#799) ;
#636 = LINE('',#3493,#800) ;
#637 = LINE('',#3494,#801) ;
#638 = LINE('',#3497,#802) ;
#639 = LINE('',#3499,#803) ;
#640 = LINE('',#3500,#804) ;
#641 = LINE('',#3502,#805) ;
#642 = LINE('',#3503,#806) ;
#643 = LINE('',#3510,#807) ;
#644 = LINE('',#3514,#808) ;
#645 = LINE('',#3518,#809) ;
#646 = LINE('',#3520,#810) ;
#647 = LINE('',#3521,#811) ;
#648 = LINE('',#3525,#812) ;
#649 = LINE('',#3529,#813) ;
#650 = LINE('',#3533,#814) ;
#651 = LINE('',#3535,#815) ;
#652 = LINE('',#3536,#816) ;
#653 = LINE('',#3539,#817) ;
#654 = LINE('',#3540,#818) ;
#655 = LINE('',#3541,#819) ;
#656 = LINE('',#3544,#820) ;
#657 = LINE('',#3545,#821) ;
#658 = LINE('',#3547,#822) ;
#659 = LINE('',#3548,#823) ;
#660 = LINE('',#3550,#824) ;
#661 = LINE('',#3553,#825) ;
#662 = LINE('',#3554,#826) ;
#663 = LINE('',#3557,#827) ;
#664 = LINE('',#3558,#828) ;
#665 = LINE('',#3560,#829) ;
#666 = LINE('',#3561,#830) ;
#667 = LINE('',#3571,#831) ;
#668 = LINE('',#3574,#832) ;
#669 = LINE('',#3577,#833) ;
#670 = LINE('',#3579,#834) ;
#671 = LINE('',#3580,#835) ;
#672 = LINE('',#3585,#836) ;
#673 = LINE('',#3588,#837) ;
#674 = LINE('',#3589,#838) ;
#675 = VECTOR('',#2417,47.5) ;
#676 = VECTOR('',#2422,1000.) ;
#677 = VECTOR('',#2423,1000.) ;
#678 = VECTOR('',#2424,1000.) ;
#679 = VECTOR('',#2425,1000.) ;
#680 = VECTOR('',#2428,1000.) ;
#681 = VECTOR('',#2429,1000.) ;
#682 = VECTOR('',#2430,1000.) ;
#683 = VECTOR('',#2433,1000.) ;
#684 = VECTOR('',#2434,1000.) ;
#685 = VECTOR('',#2435,1000.) ;
#686 = VECTOR('',#2438,1000.) ;
#687 = VECTOR('',#2439,1000.) ;
#688 = VECTOR('',#2440,1000.) ;
#689 = VECTOR('',#2445,1000.) ;
#690 = VECTOR('',#2464,6.50000000001752) ;
#691 = VECTOR('',#2471,6.50000000000472) ;
#692 = VECTOR('',#2478,6.50000000000422) ;
#693 = VECTOR('',#2485,6.50000000000406) ;
#694 = VECTOR('',#2492,6.50000000000367) ;
#695 = VECTOR('',#2499,6.50000000000261) ;
#696 = VECTOR('',#2506,6.50000000000162) ;
#697 = VECTOR('',#2513,6.50000000000089) ;
#698 = VECTOR('',#2520,6.50000000000024) ;
#699 = VECTOR('',#2527,6.49999999999945) ;
#700 = VECTOR('',#2534,6.49999999999912) ;
#701 = VECTOR('',#2541,6.49999999999901) ;
#702 = VECTOR('',#2548,6.49999999999912) ;
#703 = VECTOR('',#2555,6.49999999999928) ;
#704 = VECTOR('',#2562,6.4999999999921) ;
#705 = VECTOR('',#2569,6.50000000000001) ;
#706 = VECTOR('',#2576,285.) ;
#707 = VECTOR('',#2581,1000.) ;
#708 = VECTOR('',#2582,1000.) ;
#709 = VECTOR('',#2583,1000.) ;
#710 = VECTOR('',#2584,1000.) ;
#711 = VECTOR('',#2587,1000.) ;
#712 = VECTOR('',#2588,1000.) ;
#713 = VECTOR('',#2589,1000.) ;
#714 = VECTOR('',#2592,1000.) ;
#715 = VECTOR('',#2593,1000.) ;
#716 = VECTOR('',#2594,1000.) ;
#717 = VECTOR('',#2597,1000.) ;
#718 = VECTOR('',#2598,1000.) ;
#719 = VECTOR('',#2599,1000.) ;
#720 = VECTOR('',#2604,1000.) ;
#721 = VECTOR('',#2623,5.50000000000002) ;
#722 = VECTOR('',#2630,5.50000000000002) ;
#723 = VECTOR('',#2637,5.50000000000001) ;
#724 = VECTOR('',#2644,5.50000000000001) ;
#725 = VECTOR('',#2651,5.50000000000001) ;
#726 = VECTOR('',#2658,5.50000000000001) ;
#727 = VECTOR('',#2665,5.50000000000001) ;
#728 = VECTOR('',#2672,5.50000000000001) ;
#729 = VECTOR('',#2679,5.50000000000002) ;
#730 = VECTOR('',#2686,5.50000000000002) ;
#731 = VECTOR('',#2693,5.49999999999999) ;
#732 = VECTOR('',#2700,5.49999999999999) ;
#733 = VECTOR('',#2707,5.49999999999999) ;
#734 = VECTOR('',#2714,5.49999999999999) ;
#735 = VECTOR('',#2721,5.49999999999999) ;
#736 = VECTOR('',#2728,5.50000000000002) ;
#737 = VECTOR('',#2735,5.50000000000001) ;
#738 = VECTOR('',#2742,5.50000000000001) ;
#739 = VECTOR('',#2749,5.50000000000001) ;
#740 = VECTOR('',#2756,5.50000000000001) ;
#741 = VECTOR('',#2763,5.50000000000001) ;
#742 = VECTOR('',#2770,5.50000000000001) ;
#743 = VECTOR('',#2775,1000.) ;
#744 = VECTOR('',#2776,1000.) ;
#745 = VECTOR('',#2777,1000.) ;
#746 = VECTOR('',#2778,1000.) ;
#747 = VECTOR('',#2779,1000.) ;
#748 = VECTOR('',#2780,1000.) ;
#749 = VECTOR('',#2781,1000.) ;
#750 = VECTOR('',#2782,1000.) ;
#751 = VECTOR('',#2783,1000.) ;
#752 = VECTOR('',#2784,1000.) ;
#753 = VECTOR('',#2785,1000.) ;
#754 = VECTOR('',#2786,1000.) ;
#755 = VECTOR('',#2789,1000.) ;
#756 = VECTOR('',#2790,1000.) ;
#757 = VECTOR('',#2791,1000.) ;
#758 = VECTOR('',#2792,1000.) ;
#759 = VECTOR('',#2793,1000.) ;
#760 = VECTOR('',#2794,1000.) ;
#761 = VECTOR('',#2795,1000.) ;
#762 = VECTOR('',#2796,1000.) ;
#763 = VECTOR('',#2797,1000.) ;
#764 = VECTOR('',#2798,1000.) ;
#765 = VECTOR('',#2799,1000.) ;
#766 = VECTOR('',#2800,1000.) ;
#767 = VECTOR('',#2803,1000.) ;
#768 = VECTOR('',#2804,1000.) ;
#769 = VECTOR('',#2807,1000.) ;
#770 = VECTOR('',#2810,1000.) ;
#771 = VECTOR('',#2813,1000.) ;
#772 = VECTOR('',#2816,1000.) ;
#773 = VECTOR('',#2819,1000.) ;
#774 = VECTOR('',#2822,1000.) ;
#775 = VECTOR('',#2827,1000.) ;
#776 = VECTOR('',#2828,1000.) ;
#777 = VECTOR('',#2831,1000.) ;
#778 = VECTOR('',#2834,1000.) ;
#779 = VECTOR('',#2843,1000.) ;
#780 = VECTOR('',#2846,1000.) ;
#781 = VECTOR('',#2849,1000.) ;
#782 = VECTOR('',#2850,1000.) ;
#783 = VECTOR('',#2851,1000.) ;
#784 = VECTOR('',#2856,1000.) ;
#785 = VECTOR('',#2861,1000.) ;
#786 = VECTOR('',#2862,1000.) ;
#787 = VECTOR('',#2871,1000.) ;
#788 = VECTOR('',#2872,1000.) ;
#789 = VECTOR('',#2873,1000.) ;
#790 = VECTOR('',#2874,1000.) ;
#791 = VECTOR('',#2879,1000.) ;
#792 = VECTOR('',#2884,1000.) ;
#793 = VECTOR('',#2885,1000.) ;
#794 = VECTOR('',#2886,1000.) ;
#795 = VECTOR('',#2901,1000.) ;
#796 = VECTOR('',#2902,1000.) ;
#797 = VECTOR('',#2903,1000.) ;
#798 = VECTOR('',#2904,1000.) ;
#799 = VECTOR('',#2907,1000.) ;
#800 = VECTOR('',#2908,1000.) ;
#801 = VECTOR('',#2909,1000.) ;
#802 = VECTOR('',#2912,1000.) ;
#803 = VECTOR('',#2913,1000.) ;
#804 = VECTOR('',#2914,1000.) ;
#805 = VECTOR('',#2917,1000.) ;
#806 = VECTOR('',#2918,1000.) ;
#807 = VECTOR('',#2927,1000.) ;
#808 = VECTOR('',#2930,1000.) ;
#809 = VECTOR('',#2935,1000.) ;
#810 = VECTOR('',#2936,1000.) ;
#811 = VECTOR('',#2937,1000.) ;
#812 = VECTOR('',#2940,1000.) ;
#813 = VECTOR('',#2943,1000.) ;
#814 = VECTOR('',#2948,1000.) ;
#815 = VECTOR('',#2949,1000.) ;
#816 = VECTOR('',#2950,1000.) ;
#817 = VECTOR('',#2953,1000.) ;
#818 = VECTOR('',#2954,1000.) ;
#819 = VECTOR('',#2955,1000.) ;
#820 = VECTOR('',#2958,1000.) ;
#821 = VECTOR('',#2959,1000.) ;
#822 = VECTOR('',#2962,1000.) ;
#823 = VECTOR('',#2963,1000.) ;
#824 = VECTOR('',#2966,1000.) ;
#825 = VECTOR('',#2969,1000.) ;
#826 = VECTOR('',#2970,1000.) ;
#827 = VECTOR('',#2973,1000.) ;
#828 = VECTOR('',#2974,1000.) ;
#829 = VECTOR('',#2977,1000.) ;
#830 = VECTOR('',#2978,1000.) ;
#831 = VECTOR('',#2991,1000.) ;
#832 = VECTOR('',#2994,1000.) ;
#833 = VECTOR('',#2997,1000.) ;
#834 = VECTOR('',#2998,1000.) ;
#835 = VECTOR('',#2999,1000.) ;
#836 = VECTOR('',#3004,1000.) ;
#837 = VECTOR('',#3009,1000.) ;
#838 = VECTOR('',#3010,1000.) ;
#839 = CIRCLE('',#2183,47.5) ;
#840 = CIRCLE('',#2184,47.5) ;
#841 = CIRCLE('',#2190,790.) ;
#842 = CIRCLE('',#2191,790.) ;
#843 = CIRCLE('',#2193,465.) ;
#844 = CIRCLE('',#2194,465.) ;
#845 = CIRCLE('',#2199,6.50000000001752) ;
#846 = CIRCLE('',#2200,6.50000000001752) ;
#847 = CIRCLE('',#2202,6.50000000000472) ;
#848 = CIRCLE('',#2203,6.50000000000472) ;
#849 = CIRCLE('',#2205,6.50000000000422) ;
#850 = CIRCLE('',#2206,6.50000000000422) ;
#851 = CIRCLE('',#2208,6.50000000000406) ;
#852 = CIRCLE('',#2209,6.50000000000406) ;
#853 = CIRCLE('',#2211,6.50000000000367) ;
#854 = CIRCLE('',#2212,6.50000000000367) ;
#855 = CIRCLE('',#2214,6.50000000000261) ;
#856 = CIRCLE('',#2215,6.50000000000261) ;
#857 = CIRCLE('',#2217,6.50000000000162) ;
#858 = CIRCLE('',#2218,6.50000000000162) ;
#859 = CIRCLE('',#2220,6.50000000000089) ;
#860 = CIRCLE('',#2221,6.50000000000089) ;
#861 = CIRCLE('',#2223,6.50000000000024) ;
#862 = CIRCLE('',#2224,6.50000000000024) ;
#863 = CIRCLE('',#2226,6.49999999999945) ;
#864 = CIRCLE('',#2227,6.49999999999945) ;
#865 = CIRCLE('',#2229,6.49999999999912) ;
#866 = CIRCLE('',#2230,6.49999999999912) ;
#867 = CIRCLE('',#2232,6.49999999999901) ;
#868 = CIRCLE('',#2233,6.49999999999901) ;
#869 = CIRCLE('',#2235,6.49999999999912) ;
#870 = CIRCLE('',#2236,6.49999999999912) ;
#871 = CIRCLE('',#2238,6.49999999999928) ;
#872 = CIRCLE('',#2239,6.49999999999928) ;
#873 = CIRCLE('',#2241,6.4999999999921) ;
#874 = CIRCLE('',#2242,6.4999999999921) ;
#875 = CIRCLE('',#2244,6.50000000000001) ;
#876 = CIRCLE('',#2245,6.50000000000001) ;
#877 = CIRCLE('',#2247,285.) ;
#878 = CIRCLE('',#2248,285.) ;
#879 = CIRCLE('',#2254,790.) ;
#880 = CIRCLE('',#2255,790.) ;
#881 = CIRCLE('',#2257,465.) ;
#882 = CIRCLE('',#2258,465.) ;
#883 = CIRCLE('',#2263,5.50000000000002) ;
#884 = CIRCLE('',#2264,5.50000000000002) ;
#885 = CIRCLE('',#2266,5.50000000000002) ;
#886 = CIRCLE('',#2267,5.50000000000002) ;
#887 = CIRCLE('',#2269,5.50000000000001) ;
#888 = CIRCLE('',#2270,5.50000000000001) ;
#889 = CIRCLE('',#2272,5.50000000000001) ;
#890 = CIRCLE('',#2273,5.50000000000001) ;
#891 = CIRCLE('',#2275,5.50000000000001) ;
#892 = CIRCLE('',#2276,5.50000000000001) ;
#893 = CIRCLE('',#2278,5.50000000000001) ;
#894 = CIRCLE('',#2279,5.50000000000001) ;
#895 = CIRCLE('',#2281,5.50000000000001) ;
#896 = CIRCLE('',#2282,5.50000000000001) ;
#897 = CIRCLE('',#2284,5.50000000000001) ;
#898 = CIRCLE('',#2285,5.50000000000001) ;
#899 = CIRCLE('',#2287,5.50000000000002) ;
#900 = CIRCLE('',#2288,5.50000000000002) ;
#901 = CIRCLE('',#2290,5.50000000000002) ;
#902 = CIRCLE('',#2291,5.50000000000002) ;
#903 = CIRCLE('',#2293,5.49999999999999) ;
#904 = CIRCLE('',#2294,5.49999999999999) ;
#905 = CIRCLE('',#2296,5.49999999999999) ;
#906 = CIRCLE('',#2297,5.49999999999999) ;
#907 = CIRCLE('',#2299,5.49999999999999) ;
#908 = CIRCLE('',#2300,5.49999999999999) ;
#909 = CIRCLE('',#2302,5.49999999999999) ;
#910 = CIRCLE('',#2303,5.49999999999999) ;
#911 = CIRCLE('',#2305,5.49999999999999) ;
#912 = CIRCLE('',#2306,5.49999999999999) ;
#913 = CIRCLE('',#2308,5.50000000000002) ;
#914 = CIRCLE('',#2309,5.50000000000002) ;
#915 = CIRCLE('',#2311,5.50000000000001) ;
#916 = CIRCLE('',#2312,5.50000000000001) ;
#917 = CIRCLE('',#2314,5.50000000000001) ;
#918 = CIRCLE('',#2315,5.50000000000001) ;
#919 = CIRCLE('',#2317,5.50000000000001) ;
#920 = CIRCLE('',#2318,5.50000000000001) ;
#921 = CIRCLE('',#2320,5.50000000000001) ;
#922 = CIRCLE('',#2321,5.50000000000001) ;
#923 = CIRCLE('',#2323,5.50000000000001) ;
#924 = CIRCLE('',#2324,5.50000000000001) ;
#925 = CIRCLE('',#2326,5.50000000000001) ;
#926 = CIRCLE('',#2327,5.50000000000001) ;
#927 = CIRCLE('',#2344,780.2) ;
#928 = CIRCLE('',#2345,780.2) ;
#929 = CIRCLE('',#2348,785.) ;
#930 = CIRCLE('',#2349,785.) ;
#931 = CIRCLE('',#2356,460.) ;
#932 = CIRCLE('',#2357,460.) ;
#933 = CIRCLE('',#2360,455.2) ;
#934 = CIRCLE('',#2361,455.2) ;
#935 = CIRCLE('',#2373,26.) ;
#936 = CIRCLE('',#2374,21.2) ;
#937 = CIRCLE('',#2377,26.) ;
#938 = CIRCLE('',#2378,21.2) ;
#939 = CIRCLE('',#2392,780.2) ;
#940 = CIRCLE('',#2393,780.2) ;
#941 = CIRCLE('',#2396,785.) ;
#942 = CIRCLE('',#2397,785.) ;
#943 = VERTEX_POINT('',#3034) ;
#944 = VERTEX_POINT('',#3036) ;
#945 = VERTEX_POINT('',#3040) ;
#946 = VERTEX_POINT('',#3041) ;
#947 = VERTEX_POINT('',#3043) ;
#948 = VERTEX_POINT('',#3045) ;
#949 = VERTEX_POINT('',#3049) ;
#950 = VERTEX_POINT('',#3051) ;
#951 = VERTEX_POINT('',#3055) ;
#952 = VERTEX_POINT('',#3057) ;
#953 = VERTEX_POINT('',#3061) ;
#954 = VERTEX_POINT('',#3063) ;
#955 = VERTEX_POINT('',#3067) ;
#956 = VERTEX_POINT('',#3069) ;
#957 = VERTEX_POINT('',#3079) ;
#958 = VERTEX_POINT('',#3081) ;
#959 = VERTEX_POINT('',#3085) ;
#960 = VERTEX_POINT('',#3087) ;
#961 = VERTEX_POINT('',#3091) ;
#962 = VERTEX_POINT('',#3093) ;
#963 = VERTEX_POINT('',#3097) ;
#964 = VERTEX_POINT('',#3099) ;
#965 = VERTEX_POINT('',#3103) ;
#966 = VERTEX_POINT('',#3105) ;
#967 = VERTEX_POINT('',#3109) ;
#968 = VERTEX_POINT('',#3111) ;
#969 = VERTEX_POINT('',#3115) ;
#970 = VERTEX_POINT('',#3117) ;
#971 = VERTEX_POINT('',#3121) ;
#972 = VERTEX_POINT('',#3123) ;
#973 = VERTEX_POINT('',#3127) ;
#974 = VERTEX_POINT('',#3129) ;
#975 = VERTEX_POINT('',#3133) ;
#976 = VERTEX_POINT('',#3135) ;
#977 = VERTEX_POINT('',#3139) ;
#978 = VERTEX_POINT('',#3141) ;
#979 = VERTEX_POINT('',#3145) ;
#980 = VERTEX_POINT('',#3147) ;
#981 = VERTEX_POINT('',#3151) ;
#982 = VERTEX_POINT('',#3153) ;
#983 = VERTEX_POINT('',#3157) ;
#984 = VERTEX_POINT('',#3159) ;
#985 = VERTEX_POINT('',#3163) ;
#986 = VERTEX_POINT('',#3165) ;
#987 = VERTEX_POINT('',#3169) ;
#988 = VERTEX_POINT('',#3171) ;
#989 = VERTEX_POINT('',#3175) ;
#990 = VERTEX_POINT('',#3177) ;
#991 = VERTEX_POINT('',#3181) ;
#992 = VERTEX_POINT('',#3182) ;
#993 = VERTEX_POINT('',#3184) ;
#994 = VERTEX_POINT('',#3186) ;
#995 = VERTEX_POINT('',#3190) ;
#996 = VERTEX_POINT('',#3192) ;
#997 = VERTEX_POINT('',#3196) ;
#998 = VERTEX_POINT('',#3198) ;
#999 = VERTEX_POINT('',#3202) ;
#1000 = VERTEX_POINT('',#3204) ;
#1001 = VERTEX_POINT('',#3208) ;
#1002 = VERTEX_POINT('',#3210) ;
#1003 = VERTEX_POINT('',#3220) ;
#1004 = VERTEX_POINT('',#3222) ;
#1005 = VERTEX_POINT('',#3226) ;
#1006 = VERTEX_POINT('',#3228) ;
#1007 = VERTEX_POINT('',#3232) ;
#1008 = VERTEX_POINT('',#3234) ;
#1009 = VERTEX_POINT('',#3238) ;
#1010 = VERTEX_POINT('',#3240) ;
#1011 = VERTEX_POINT('',#3244) ;
#1012 = VERTEX_POINT('',#3246) ;
#1013 = VERTEX_POINT('',#3250) ;
#1014 = VERTEX_POINT('',#3252) ;
#1015 = VERTEX_POINT('',#3256) ;
#1016 = VERTEX_POINT('',#3258) ;
#1017 = VERTEX_POINT('',#3262) ;
#1018 = VERTEX_POINT('',#3264) ;
#1019 = VERTEX_POINT('',#3268) ;
#1020 = VERTEX_POINT('',#3270) ;
#1021 = VERTEX_POINT('',#3274) ;
#1022 = VERTEX_POINT('',#3276) ;
#1023 = VERTEX_POINT('',#3280) ;
#1024 = VERTEX_POINT('',#3282) ;
#1025 = VERTEX_POINT('',#3286) ;
#1026 = VERTEX_POINT('',#3288) ;
#1027 = VERTEX_POINT('',#3292) ;
#1028 = VERTEX_POINT('',#3294) ;
#1029 = VERTEX_POINT('',#3298) ;
#1030 = VERTEX_POINT('',#3300) ;
#1031 = VERTEX_POINT('',#3304) ;
#1032 = VERTEX_POINT('',#3306) ;
#1033 = VERTEX_POINT('',#3310) ;
#1034 = VERTEX_POINT('',#3312) ;
#1035 = VERTEX_POINT('',#3316) ;
#1036 = VERTEX_POINT('',#3318) ;
#1037 = VERTEX_POINT('',#3322) ;
#1038 = VERTEX_POINT('',#3324) ;
#1039 = VERTEX_POINT('',#3328) ;
#1040 = VERTEX_POINT('',#3330) ;
#1041 = VERTEX_POINT('',#3334) ;
#1042 = VERTEX_POINT('',#3336) ;
#1043 = VERTEX_POINT('',#3340) ;
#1044 = VERTEX_POINT('',#3342) ;
#1045 = VERTEX_POINT('',#3346) ;
#1046 = VERTEX_POINT('',#3348) ;
#1047 = VERTEX_POINT('',#3352) ;
#1048 = VERTEX_POINT('',#3353) ;
#1049 = VERTEX_POINT('',#3355) ;
#1050 = VERTEX_POINT('',#3357) ;
#1051 = VERTEX_POINT('',#3359) ;
#1052 = VERTEX_POINT('',#3361) ;
#1053 = VERTEX_POINT('',#3363) ;
#1054 = VERTEX_POINT('',#3365) ;
#1055 = VERTEX_POINT('',#3368) ;
#1056 = VERTEX_POINT('',#3369) ;
#1057 = VERTEX_POINT('',#3371) ;
#1058 = VERTEX_POINT('',#3373) ;
#1059 = VERTEX_POINT('',#3377) ;
#1060 = VERTEX_POINT('',#3378) ;
#1061 = VERTEX_POINT('',#3380) ;
#1062 = VERTEX_POINT('',#3382) ;
#1063 = VERTEX_POINT('',#3384) ;
#1064 = VERTEX_POINT('',#3386) ;
#1065 = VERTEX_POINT('',#3388) ;
#1066 = VERTEX_POINT('',#3390) ;
#1067 = VERTEX_POINT('',#3393) ;
#1068 = VERTEX_POINT('',#3394) ;
#1069 = VERTEX_POINT('',#3396) ;
#1070 = VERTEX_POINT('',#3398) ;
#1071 = VERTEX_POINT('',#3427) ;
#1072 = VERTEX_POINT('',#3428) ;
#1073 = VERTEX_POINT('',#3430) ;
#1074 = VERTEX_POINT('',#3432) ;
#1075 = VERTEX_POINT('',#3436) ;
#1076 = VERTEX_POINT('',#3438) ;
#1077 = VERTEX_POINT('',#3442) ;
#1078 = VERTEX_POINT('',#3444) ;
#1079 = VERTEX_POINT('',#3454) ;
#1080 = VERTEX_POINT('',#3455) ;
#1081 = VERTEX_POINT('',#3457) ;
#1082 = VERTEX_POINT('',#3459) ;
#1083 = VERTEX_POINT('',#3463) ;
#1084 = VERTEX_POINT('',#3465) ;
#1085 = VERTEX_POINT('',#3469) ;
#1086 = VERTEX_POINT('',#3471) ;
#1087 = VERTEX_POINT('',#3481) ;
#1088 = VERTEX_POINT('',#3482) ;
#1089 = VERTEX_POINT('',#3484) ;
#1090 = VERTEX_POINT('',#3486) ;
#1091 = VERTEX_POINT('',#3490) ;
#1092 = VERTEX_POINT('',#3492) ;
#1093 = VERTEX_POINT('',#3496) ;
#1094 = VERTEX_POINT('',#3498) ;
#1095 = VERTEX_POINT('',#3508) ;
#1096 = VERTEX_POINT('',#3509) ;
#1097 = VERTEX_POINT('',#3511) ;
#1098 = VERTEX_POINT('',#3513) ;
#1099 = VERTEX_POINT('',#3517) ;
#1100 = VERTEX_POINT('',#3519) ;
#1101 = VERTEX_POINT('',#3523) ;
#1102 = VERTEX_POINT('',#3524) ;
#1103 = VERTEX_POINT('',#3526) ;
#1104 = VERTEX_POINT('',#3528) ;
#1105 = VERTEX_POINT('',#3532) ;
#1106 = VERTEX_POINT('',#3534) ;
#1107 = VERTEX_POINT('',#3538) ;
#1108 = VERTEX_POINT('',#3543) ;
#1109 = VERTEX_POINT('',#3552) ;
#1110 = VERTEX_POINT('',#3556) ;
#1111 = VERTEX_POINT('',#3567) ;
#1112 = VERTEX_POINT('',#3568) ;
#1113 = VERTEX_POINT('',#3570) ;
#1114 = VERTEX_POINT('',#3572) ;
#1115 = VERTEX_POINT('',#3576) ;
#1116 = VERTEX_POINT('',#3578) ;
#1117 = VERTEX_POINT('',#3582) ;
#1118 = VERTEX_POINT('',#3584) ;
#1119 = EDGE_CURVE('',#943,#943,#839,.T.) ;
#1120 = EDGE_CURVE('',#943,#944,#511,.T.) ;
#1121 = EDGE_CURVE('',#944,#944,#840,.T.) ;
#1122 = EDGE_CURVE('',#945,#946,#512,.T.) ;
#1123 = EDGE_CURVE('',#947,#945,#513,.T.) ;
#1124 = EDGE_CURVE('',#947,#948,#514,.T.) ;
#1125 = EDGE_CURVE('',#948,#946,#515,.T.) ;
#1126 = EDGE_CURVE('',#949,#945,#516,.T.) ;
#1127 = EDGE_CURVE('',#950,#949,#517,.T.) ;
#1128 = EDGE_CURVE('',#950,#947,#518,.T.) ;
#1129 = EDGE_CURVE('',#951,#949,#519,.T.) ;
#1130 = EDGE_CURVE('',#952,#951,#520,.T.) ;
#1131 = EDGE_CURVE('',#952,#950,#521,.T.) ;
#1132 = EDGE_CURVE('',#953,#951,#522,.T.) ;
#1133 = EDGE_CURVE('',#954,#953,#523,.T.) ;
#1134 = EDGE_CURVE('',#954,#952,#524,.T.) ;
#1135 = EDGE_CURVE('',#955,#953,#841,.T.) ;
#1136 = EDGE_CURVE('',#956,#955,#525,.T.) ;
#1137 = EDGE_CURVE('',#956,#954,#842,.T.) ;
#1138 = EDGE_CURVE('',#946,#955,#843,.T.) ;
#1139 = EDGE_CURVE('',#948,#956,#844,.T.) ;
#1140 = EDGE_CURVE('',#957,#957,#845,.T.) ;
#1141 = EDGE_CURVE('',#957,#958,#526,.T.) ;
#1142 = EDGE_CURVE('',#958,#958,#846,.T.) ;
#1143 = EDGE_CURVE('',#959,#959,#847,.T.) ;
#1144 = EDGE_CURVE('',#959,#960,#527,.T.) ;
#1145 = EDGE_CURVE('',#960,#960,#848,.T.) ;
#1146 = EDGE_CURVE('',#961,#961,#849,.T.) ;
#1147 = EDGE_CURVE('',#961,#962,#528,.T.) ;
#1148 = EDGE_CURVE('',#962,#962,#850,.T.) ;
#1149 = EDGE_CURVE('',#963,#963,#851,.T.) ;
#1150 = EDGE_CURVE('',#963,#964,#529,.T.) ;
#1151 = EDGE_CURVE('',#964,#964,#852,.T.) ;
#1152 = EDGE_CURVE('',#965,#965,#853,.T.) ;
#1153 = EDGE_CURVE('',#965,#966,#530,.T.) ;
#1154 = EDGE_CURVE('',#966,#966,#854,.T.) ;
#1155 = EDGE_CURVE('',#967,#967,#855,.T.) ;
#1156 = EDGE_CURVE('',#967,#968,#531,.T.) ;
#1157 = EDGE_CURVE('',#968,#968,#856,.T.) ;
#1158 = EDGE_CURVE('',#969,#969,#857,.T.) ;
#1159 = EDGE_CURVE('',#969,#970,#532,.T.) ;
#1160 = EDGE_CURVE('',#970,#970,#858,.T.) ;
#1161 = EDGE_CURVE('',#971,#971,#859,.T.) ;
#1162 = EDGE_CURVE('',#971,#972,#533,.T.) ;
#1163 = EDGE_CURVE('',#972,#972,#860,.T.) ;
#1164 = EDGE_CURVE('',#973,#973,#861,.T.) ;
#1165 = EDGE_CURVE('',#973,#974,#534,.T.) ;
#1166 = EDGE_CURVE('',#974,#974,#862,.T.) ;
#1167 = EDGE_CURVE('',#975,#975,#863,.T.) ;
#1168 = EDGE_CURVE('',#975,#976,#535,.T.) ;
#1169 = EDGE_CURVE('',#976,#976,#864,.T.) ;
#1170 = EDGE_CURVE('',#977,#977,#865,.T.) ;
#1171 = EDGE_CURVE('',#977,#978,#536,.T.) ;
#1172 = EDGE_CURVE('',#978,#978,#866,.T.) ;
#1173 = EDGE_CURVE('',#979,#979,#867,.T.) ;
#1174 = EDGE_CURVE('',#979,#980,#537,.T.) ;
#1175 = EDGE_CURVE('',#980,#980,#868,.T.) ;
#1176 = EDGE_CURVE('',#981,#981,#869,.T.) ;
#1177 = EDGE_CURVE('',#981,#982,#538,.T.) ;
#1178 = EDGE_CURVE('',#982,#982,#870,.T.) ;
#1179 = EDGE_CURVE('',#983,#983,#871,.T.) ;
#1180 = EDGE_CURVE('',#983,#984,#539,.T.) ;
#1181 = EDGE_CURVE('',#984,#984,#872,.T.) ;
#1182 = EDGE_CURVE('',#985,#985,#873,.T.) ;
#1183 = EDGE_CURVE('',#985,#986,#540,.T.) ;
#1184 = EDGE_CURVE('',#986,#986,#874,.T.) ;
#1185 = EDGE_CURVE('',#987,#987,#875,.T.) ;
#1186 = EDGE_CURVE('',#987,#988,#541,.T.) ;
#1187 = EDGE_CURVE('',#988,#988,#876,.T.) ;
#1188 = EDGE_CURVE('',#989,#989,#877,.T.) ;
#1189 = EDGE_CURVE('',#989,#990,#542,.T.) ;
#1190 = EDGE_CURVE('',#990,#990,#878,.T.) ;
#1191 = EDGE_CURVE('',#991,#992,#543,.T.) ;
#1192 = EDGE_CURVE('',#993,#991,#544,.T.) ;
#1193 = EDGE_CURVE('',#993,#994,#545,.T.) ;
#1194 = EDGE_CURVE('',#994,#992,#546,.T.) ;
#1195 = EDGE_CURVE('',#995,#991,#547,.T.) ;
#1196 = EDGE_CURVE('',#996,#995,#548,.T.) ;
#1197 = EDGE_CURVE('',#996,#993,#549,.T.) ;
#1198 = EDGE_CURVE('',#997,#995,#550,.T.) ;
#1199 = EDGE_CURVE('',#998,#997,#551,.T.) ;
#1200 = EDGE_CURVE('',#998,#996,#552,.T.) ;
#1201 = EDGE_CURVE('',#999,#997,#553,.T.) ;
#1202 = EDGE_CURVE('',#1000,#999,#554,.T.) ;
#1203 = EDGE_CURVE('',#1000,#998,#555,.T.) ;
#1204 = EDGE_CURVE('',#1001,#999,#879,.T.) ;
#1205 = EDGE_CURVE('',#1002,#1001,#556,.T.) ;
#1206 = EDGE_CURVE('',#1002,#1000,#880,.T.) ;
#1207 = EDGE_CURVE('',#992,#1001,#881,.T.) ;
#1208 = EDGE_CURVE('',#994,#1002,#882,.T.) ;
#1209 = EDGE_CURVE('',#1003,#1003,#883,.T.) ;
#1210 = EDGE_CURVE('',#1003,#1004,#557,.T.) ;
#1211 = EDGE_CURVE('',#1004,#1004,#884,.T.) ;
#1212 = EDGE_CURVE('',#1005,#1005,#885,.T.) ;
#1213 = EDGE_CURVE('',#1005,#1006,#558,.T.) ;
#1214 = EDGE_CURVE('',#1006,#1006,#886,.T.) ;
#1215 = EDGE_CURVE('',#1007,#1007,#887,.T.) ;
#1216 = EDGE_CURVE('',#1007,#1008,#559,.T.) ;
#1217 = EDGE_CURVE('',#1008,#1008,#888,.T.) ;
#1218 = EDGE_CURVE('',#1009,#1009,#889,.T.) ;
#1219 = EDGE_CURVE('',#1009,#1010,#560,.T.) ;
#1220 = EDGE_CURVE('',#1010,#1010,#890,.T.) ;
#1221 = EDGE_CURVE('',#1011,#1011,#891,.T.) ;
#1222 = EDGE_CURVE('',#1011,#1012,#561,.T.) ;
#1223 = EDGE_CURVE('',#1012,#1012,#892,.T.) ;
#1224 = EDGE_CURVE('',#1013,#1013,#893,.T.) ;
#1225 = EDGE_CURVE('',#1013,#1014,#562,.T.) ;
#1226 = EDGE_CURVE('',#1014,#1014,#894,.T.) ;
#1227 = EDGE_CURVE('',#1015,#1015,#895,.T.) ;
#1228 = EDGE_CURVE('',#1015,#1016,#563,.T.) ;
#1229 = EDGE_CURVE('',#1016,#1016,#896,.T.) ;
#1230 = EDGE_CURVE('',#1017,#1017,#897,.T.) ;
#1231 = EDGE_CURVE('',#1017,#1018,#564,.T.) ;
#1232 = EDGE_CURVE('',#1018,#1018,#898,.T.) ;
#1233 = EDGE_CURVE('',#1019,#1019,#899,.T.) ;
#1234 = EDGE_CURVE('',#1019,#1020,#565,.T.) ;
#1235 = EDGE_CURVE('',#1020,#1020,#900,.T.) ;
#1236 = EDGE_CURVE('',#1021,#1021,#901,.T.) ;
#1237 = EDGE_CURVE('',#1021,#1022,#566,.T.) ;
#1238 = EDGE_CURVE('',#1022,#1022,#902,.T.) ;
#1239 = EDGE_CURVE('',#1023,#1023,#903,.T.) ;
#1240 = EDGE_CURVE('',#1023,#1024,#567,.T.) ;
#1241 = EDGE_CURVE('',#1024,#1024,#904,.T.) ;
#1242 = EDGE_CURVE('',#1025,#1025,#905,.T.) ;
#1243 = EDGE_CURVE('',#1025,#1026,#568,.T.) ;
#1244 = EDGE_CURVE('',#1026,#1026,#906,.T.) ;
#1245 = EDGE_CURVE('',#1027,#1027,#907,.T.) ;
#1246 = EDGE_CURVE('',#1027,#1028,#569,.T.) ;
#1247 = EDGE_CURVE('',#1028,#1028,#908,.T.) ;
#1248 = EDGE_CURVE('',#1029,#1029,#909,.T.) ;
#1249 = EDGE_CURVE('',#1029,#1030,#570,.T.) ;
#1250 = EDGE_CURVE('',#1030,#1030,#910,.T.) ;
#1251 = EDGE_CURVE('',#1031,#1031,#911,.T.) ;
#1252 = EDGE_CURVE('',#1031,#1032,#571,.T.) ;
#1253 = EDGE_CURVE('',#1032,#1032,#912,.T.) ;
#1254 = EDGE_CURVE('',#1033,#1033,#913,.T.) ;
#1255 = EDGE_CURVE('',#1033,#1034,#572,.T.) ;
#1256 = EDGE_CURVE('',#1034,#1034,#914,.T.) ;
#1257 = EDGE_CURVE('',#1035,#1035,#915,.T.) ;
#1258 = EDGE_CURVE('',#1035,#1036,#573,.T.) ;
#1259 = EDGE_CURVE('',#1036,#1036,#916,.T.) ;
#1260 = EDGE_CURVE('',#1037,#1037,#917,.T.) ;
#1261 = EDGE_CURVE('',#1037,#1038,#574,.T.) ;
#1262 = EDGE_CURVE('',#1038,#1038,#918,.T.) ;
#1263 = EDGE_CURVE('',#1039,#1039,#919,.T.) ;
#1264 = EDGE_CURVE('',#1039,#1040,#575,.T.) ;
#1265 = EDGE_CURVE('',#1040,#1040,#920,.T.) ;
#1266 = EDGE_CURVE('',#1041,#1041,#921,.T.) ;
#1267 = EDGE_CURVE('',#1041,#1042,#576,.T.) ;
#1268 = EDGE_CURVE('',#1042,#1042,#922,.T.) ;
#1269 = EDGE_CURVE('',#1043,#1043,#923,.T.) ;
#1270 = EDGE_CURVE('',#1043,#1044,#577,.T.) ;
#1271 = EDGE_CURVE('',#1044,#1044,#924,.T.) ;
#1272 = EDGE_CURVE('',#1045,#1045,#925,.T.) ;
#1273 = EDGE_CURVE('',#1045,#1046,#578,.T.) ;
#1274 = EDGE_CURVE('',#1046,#1046,#926,.T.) ;
#1275 = EDGE_CURVE('',#1047,#1048,#579,.T.) ;
#1276 = EDGE_CURVE('',#1048,#1049,#580,.T.) ;
#1277 = EDGE_CURVE('',#1049,#1050,#581,.T.) ;
#1278 = EDGE_CURVE('',#1050,#1051,#582,.T.) ;
#1279 = EDGE_CURVE('',#1051,#1052,#583,.T.) ;
#1280 = EDGE_CURVE('',#1052,#1053,#584,.T.) ;
#1281 = EDGE_CURVE('',#1053,#1054,#585,.T.) ;
#1282 = EDGE_CURVE('',#1054,#1047,#586,.T.) ;
#1283 = EDGE_CURVE('',#1055,#1056,#587,.T.) ;
#1284 = EDGE_CURVE('',#1057,#1055,#588,.T.) ;
#1285 = EDGE_CURVE('',#1058,#1057,#589,.T.) ;
#1286 = EDGE_CURVE('',#1056,#1058,#590,.T.) ;
#1287 = EDGE_CURVE('',#1059,#1060,#591,.T.) ;
#1288 = EDGE_CURVE('',#1061,#1059,#592,.T.) ;
#1289 = EDGE_CURVE('',#1062,#1061,#593,.T.) ;
#1290 = EDGE_CURVE('',#1063,#1062,#594,.T.) ;
#1291 = EDGE_CURVE('',#1064,#1063,#595,.T.) ;
#1292 = EDGE_CURVE('',#1065,#1064,#596,.T.) ;
#1293 = EDGE_CURVE('',#1066,#1065,#597,.T.) ;
#1294 = EDGE_CURVE('',#1060,#1066,#598,.T.) ;
#1295 = EDGE_CURVE('',#1067,#1068,#599,.T.) ;
#1296 = EDGE_CURVE('',#1068,#1069,#600,.T.) ;
#1297 = EDGE_CURVE('',#1069,#1070,#601,.T.) ;
#1298 = EDGE_CURVE('',#1070,#1067,#602,.T.) ;
#1299 = EDGE_CURVE('',#1048,#1060,#603,.T.) ;
#1300 = EDGE_CURVE('',#1047,#1059,#604,.T.) ;
#1301 = EDGE_CURVE('',#1049,#1066,#605,.T.) ;
#1302 = EDGE_CURVE('',#1050,#1065,#606,.T.) ;
#1303 = EDGE_CURVE('',#1051,#1064,#607,.T.) ;
#1304 = EDGE_CURVE('',#1052,#1063,#608,.T.) ;
#1305 = EDGE_CURVE('',#1053,#1062,#609,.T.) ;
#1306 = EDGE_CURVE('',#1054,#1061,#610,.T.) ;
#1307 = EDGE_CURVE('',#1057,#1067,#611,.T.) ;
#1308 = EDGE_CURVE('',#1055,#1068,#612,.T.) ;
#1309 = EDGE_CURVE('',#1056,#1069,#613,.T.) ;
#1310 = EDGE_CURVE('',#1058,#1070,#614,.T.) ;
#1311 = EDGE_CURVE('',#1071,#1072,#927,.T.) ;
#1312 = EDGE_CURVE('',#1073,#1072,#615,.T.) ;
#1313 = EDGE_CURVE('',#1074,#1073,#928,.T.) ;
#1314 = EDGE_CURVE('',#1074,#1071,#616,.T.) ;
#1315 = EDGE_CURVE('',#1075,#1072,#617,.T.) ;
#1316 = EDGE_CURVE('',#1076,#1075,#618,.T.) ;
#1317 = EDGE_CURVE('',#1076,#1073,#619,.T.) ;
#1318 = EDGE_CURVE('',#1077,#1075,#929,.T.) ;
#1319 = EDGE_CURVE('',#1078,#1077,#620,.T.) ;
#1320 = EDGE_CURVE('',#1078,#1076,#930,.T.) ;
#1321 = EDGE_CURVE('',#1071,#1077,#621,.T.) ;
#1322 = EDGE_CURVE('',#1074,#1078,#622,.T.) ;
#1323 = EDGE_CURVE('',#1079,#1080,#623,.T.) ;
#1324 = EDGE_CURVE('',#1081,#1079,#624,.T.) ;
#1325 = EDGE_CURVE('',#1081,#1082,#625,.T.) ;
#1326 = EDGE_CURVE('',#1082,#1080,#626,.T.) ;
#1327 = EDGE_CURVE('',#1083,#1079,#931,.T.) ;
#1328 = EDGE_CURVE('',#1084,#1083,#627,.T.) ;
#1329 = EDGE_CURVE('',#1084,#1081,#932,.T.) ;
#1330 = EDGE_CURVE('',#1085,#1083,#628,.T.) ;
#1331 = EDGE_CURVE('',#1086,#1085,#629,.T.) ;
#1332 = EDGE_CURVE('',#1086,#1084,#630,.T.) ;
#1333 = EDGE_CURVE('',#1085,#1080,#933,.T.) ;
#1334 = EDGE_CURVE('',#1086,#1082,#934,.T.) ;
#1335 = EDGE_CURVE('',#1087,#1088,#631,.T.) ;
#1336 = EDGE_CURVE('',#1089,#1087,#632,.T.) ;
#1337 = EDGE_CURVE('',#1089,#1090,#633,.T.) ;
#1338 = EDGE_CURVE('',#1090,#1088,#634,.T.) ;
#1339 = EDGE_CURVE('',#1091,#1087,#635,.T.) ;
#1340 = EDGE_CURVE('',#1092,#1091,#636,.T.) ;
#1341 = EDGE_CURVE('',#1092,#1089,#637,.T.) ;
#1342 = EDGE_CURVE('',#1093,#1091,#638,.T.) ;
#1343 = EDGE_CURVE('',#1094,#1093,#639,.T.) ;
#1344 = EDGE_CURVE('',#1094,#1092,#640,.T.) ;
#1345 = EDGE_CURVE('',#1088,#1093,#641,.T.) ;
#1346 = EDGE_CURVE('',#1090,#1094,#642,.T.) ;
#1347 = EDGE_CURVE('',#1095,#1096,#643,.T.) ;
#1348 = EDGE_CURVE('',#1097,#1095,#935,.T.) ;
#1349 = EDGE_CURVE('',#1098,#1097,#644,.T.) ;
#1350 = EDGE_CURVE('',#1098,#1096,#936,.T.) ;
#1351 = EDGE_CURVE('',#1095,#1099,#645,.T.) ;
#1352 = EDGE_CURVE('',#1096,#1100,#646,.T.) ;
#1353 = EDGE_CURVE('',#1099,#1100,#647,.T.) ;
#1354 = EDGE_CURVE('',#1101,#1102,#648,.T.) ;
#1355 = EDGE_CURVE('',#1101,#1103,#937,.T.) ;
#1356 = EDGE_CURVE('',#1104,#1103,#649,.T.) ;
#1357 = EDGE_CURVE('',#1102,#1104,#938,.T.) ;
#1358 = EDGE_CURVE('',#1105,#1101,#650,.T.) ;
#1359 = EDGE_CURVE('',#1106,#1102,#651,.T.) ;
#1360 = EDGE_CURVE('',#1106,#1105,#652,.T.) ;
#1361 = EDGE_CURVE('',#1104,#1107,#653,.T.) ;
#1362 = EDGE_CURVE('',#1100,#1107,#654,.T.) ;
#1363 = EDGE_CURVE('',#1096,#1104,#655,.T.) ;
#1364 = EDGE_CURVE('',#1108,#1107,#656,.T.) ;
#1365 = EDGE_CURVE('',#1099,#1108,#657,.T.) ;
#1366 = EDGE_CURVE('',#1103,#1108,#658,.T.) ;
#1367 = EDGE_CURVE('',#1095,#1103,#659,.T.) ;
#1368 = EDGE_CURVE('',#1097,#1101,#660,.T.) ;
#1369 = EDGE_CURVE('',#1109,#1105,#661,.T.) ;
#1370 = EDGE_CURVE('',#1109,#1097,#662,.T.) ;
#1371 = EDGE_CURVE('',#1110,#1106,#663,.T.) ;
#1372 = EDGE_CURVE('',#1110,#1109,#664,.T.) ;
#1373 = EDGE_CURVE('',#1098,#1102,#665,.T.) ;
#1374 = EDGE_CURVE('',#1110,#1098,#666,.T.) ;
#1375 = EDGE_CURVE('',#1111,#1112,#939,.T.) ;
#1376 = EDGE_CURVE('',#1113,#1112,#667,.T.) ;
#1377 = EDGE_CURVE('',#1114,#1113,#940,.T.) ;
#1378 = EDGE_CURVE('',#1114,#1111,#668,.T.) ;
#1379 = EDGE_CURVE('',#1115,#1112,#669,.T.) ;
#1380 = EDGE_CURVE('',#1116,#1115,#670,.T.) ;
#1381 = EDGE_CURVE('',#1116,#1113,#671,.T.) ;
#1382 = EDGE_CURVE('',#1117,#1115,#941,.T.) ;
#1383 = EDGE_CURVE('',#1118,#1117,#672,.T.) ;
#1384 = EDGE_CURVE('',#1118,#1116,#942,.T.) ;
#1385 = EDGE_CURVE('',#1111,#1117,#673,.T.) ;
#1386 = EDGE_CURVE('',#1114,#1118,#674,.T.) ;
#1387 = ORIENTED_EDGE('',*,*,#1119,.F.) ;
#1388 = ORIENTED_EDGE('',*,*,#1120,.T.) ;
#1389 = ORIENTED_EDGE('',*,*,#1121,.T.) ;
#1390 = ORIENTED_EDGE('',*,*,#1120,.F.) ;
#1391 = ORIENTED_EDGE('',*,*,#1122,.F.) ;
#1392 = ORIENTED_EDGE('',*,*,#1123,.F.) ;
#1393 = ORIENTED_EDGE('',*,*,#1124,.T.) ;
#1394 = ORIENTED_EDGE('',*,*,#1125,.T.) ;
#1395 = ORIENTED_EDGE('',*,*,#1126,.F.) ;
#1396 = ORIENTED_EDGE('',*,*,#1127,.F.) ;
#1397 = ORIENTED_EDGE('',*,*,#1128,.T.) ;
#1398 = ORIENTED_EDGE('',*,*,#1123,.T.) ;
#1399 = ORIENTED_EDGE('',*,*,#1129,.F.) ;
#1400 = ORIENTED_EDGE('',*,*,#1130,.F.) ;
#1401 = ORIENTED_EDGE('',*,*,#1131,.T.) ;
#1402 = ORIENTED_EDGE('',*,*,#1127,.T.) ;
#1403 = ORIENTED_EDGE('',*,*,#1132,.F.) ;
#1404 = ORIENTED_EDGE('',*,*,#1133,.F.) ;
#1405 = ORIENTED_EDGE('',*,*,#1134,.T.) ;
#1406 = ORIENTED_EDGE('',*,*,#1130,.T.) ;
#1407 = ORIENTED_EDGE('',*,*,#1135,.F.) ;
#1408 = ORIENTED_EDGE('',*,*,#1136,.F.) ;
#1409 = ORIENTED_EDGE('',*,*,#1137,.T.) ;
#1410 = ORIENTED_EDGE('',*,*,#1133,.T.) ;
#1411 = ORIENTED_EDGE('',*,*,#1138,.F.) ;
#1412 = ORIENTED_EDGE('',*,*,#1125,.F.) ;
#1413 = ORIENTED_EDGE('',*,*,#1139,.T.) ;
#1414 = ORIENTED_EDGE('',*,*,#1136,.T.) ;
#1415 = ORIENTED_EDGE('',*,*,#1124,.F.) ;
#1416 = ORIENTED_EDGE('',*,*,#1128,.F.) ;
#1417 = ORIENTED_EDGE('',*,*,#1131,.F.) ;
#1418 = ORIENTED_EDGE('',*,*,#1134,.F.) ;
#1419 = ORIENTED_EDGE('',*,*,#1137,.F.) ;
#1420 = ORIENTED_EDGE('',*,*,#1139,.F.) ;
#1421 = ORIENTED_EDGE('',*,*,#1119,.T.) ;
#1422 = ORIENTED_EDGE('',*,*,#1122,.T.) ;
#1423 = ORIENTED_EDGE('',*,*,#1138,.T.) ;
#1424 = ORIENTED_EDGE('',*,*,#1135,.T.) ;
#1425 = ORIENTED_EDGE('',*,*,#1132,.T.) ;
#1426 = ORIENTED_EDGE('',*,*,#1129,.T.) ;
#1427 = ORIENTED_EDGE('',*,*,#1126,.T.) ;
#1428 = ORIENTED_EDGE('',*,*,#1121,.F.) ;
#1429 = ORIENTED_EDGE('',*,*,#1140,.F.) ;
#1430 = ORIENTED_EDGE('',*,*,#1141,.T.) ;
#1431 = ORIENTED_EDGE('',*,*,#1142,.T.) ;
#1432 = ORIENTED_EDGE('',*,*,#1141,.F.) ;
#1433 = ORIENTED_EDGE('',*,*,#1143,.F.) ;
#1434 = ORIENTED_EDGE('',*,*,#1144,.T.) ;
#1435 = ORIENTED_EDGE('',*,*,#1145,.T.) ;
#1436 = ORIENTED_EDGE('',*,*,#1144,.F.) ;
#1437 = ORIENTED_EDGE('',*,*,#1146,.F.) ;
#1438 = ORIENTED_EDGE('',*,*,#1147,.T.) ;
#1439 = ORIENTED_EDGE('',*,*,#1148,.T.) ;
#1440 = ORIENTED_EDGE('',*,*,#1147,.F.) ;
#1441 = ORIENTED_EDGE('',*,*,#1149,.F.) ;
#1442 = ORIENTED_EDGE('',*,*,#1150,.T.) ;
#1443 = ORIENTED_EDGE('',*,*,#1151,.T.) ;
#1444 = ORIENTED_EDGE('',*,*,#1150,.F.) ;
#1445 = ORIENTED_EDGE('',*,*,#1152,.F.) ;
#1446 = ORIENTED_EDGE('',*,*,#1153,.T.) ;
#1447 = ORIENTED_EDGE('',*,*,#1154,.T.) ;
#1448 = ORIENTED_EDGE('',*,*,#1153,.F.) ;
#1449 = ORIENTED_EDGE('',*,*,#1155,.F.) ;
#1450 = ORIENTED_EDGE('',*,*,#1156,.T.) ;
#1451 = ORIENTED_EDGE('',*,*,#1157,.T.) ;
#1452 = ORIENTED_EDGE('',*,*,#1156,.F.) ;
#1453 = ORIENTED_EDGE('',*,*,#1158,.F.) ;
#1454 = ORIENTED_EDGE('',*,*,#1159,.T.) ;
#1455 = ORIENTED_EDGE('',*,*,#1160,.T.) ;
#1456 = ORIENTED_EDGE('',*,*,#1159,.F.) ;
#1457 = ORIENTED_EDGE('',*,*,#1161,.F.) ;
#1458 = ORIENTED_EDGE('',*,*,#1162,.T.) ;
#1459 = ORIENTED_EDGE('',*,*,#1163,.T.) ;
#1460 = ORIENTED_EDGE('',*,*,#1162,.F.) ;
#1461 = ORIENTED_EDGE('',*,*,#1164,.F.) ;
#1462 = ORIENTED_EDGE('',*,*,#1165,.T.) ;
#1463 = ORIENTED_EDGE('',*,*,#1166,.T.) ;
#1464 = ORIENTED_EDGE('',*,*,#1165,.F.) ;
#1465 = ORIENTED_EDGE('',*,*,#1167,.F.) ;
#1466 = ORIENTED_EDGE('',*,*,#1168,.T.) ;
#1467 = ORIENTED_EDGE('',*,*,#1169,.T.) ;
#1468 = ORIENTED_EDGE('',*,*,#1168,.F.) ;
#1469 = ORIENTED_EDGE('',*,*,#1170,.F.) ;
#1470 = ORIENTED_EDGE('',*,*,#1171,.T.) ;
#1471 = ORIENTED_EDGE('',*,*,#1172,.T.) ;
#1472 = ORIENTED_EDGE('',*,*,#1171,.F.) ;
#1473 = ORIENTED_EDGE('',*,*,#1173,.F.) ;
#1474 = ORIENTED_EDGE('',*,*,#1174,.T.) ;
#1475 = ORIENTED_EDGE('',*,*,#1175,.T.) ;
#1476 = ORIENTED_EDGE('',*,*,#1174,.F.) ;
#1477 = ORIENTED_EDGE('',*,*,#1176,.F.) ;
#1478 = ORIENTED_EDGE('',*,*,#1177,.T.) ;
#1479 = ORIENTED_EDGE('',*,*,#1178,.T.) ;
#1480 = ORIENTED_EDGE('',*,*,#1177,.F.) ;
#1481 = ORIENTED_EDGE('',*,*,#1179,.F.) ;
#1482 = ORIENTED_EDGE('',*,*,#1180,.T.) ;
#1483 = ORIENTED_EDGE('',*,*,#1181,.T.) ;
#1484 = ORIENTED_EDGE('',*,*,#1180,.F.) ;
#1485 = ORIENTED_EDGE('',*,*,#1182,.F.) ;
#1486 = ORIENTED_EDGE('',*,*,#1183,.T.) ;
#1487 = ORIENTED_EDGE('',*,*,#1184,.T.) ;
#1488 = ORIENTED_EDGE('',*,*,#1183,.F.) ;
#1489 = ORIENTED_EDGE('',*,*,#1185,.F.) ;
#1490 = ORIENTED_EDGE('',*,*,#1186,.T.) ;
#1491 = ORIENTED_EDGE('',*,*,#1187,.T.) ;
#1492 = ORIENTED_EDGE('',*,*,#1186,.F.) ;
#1493 = ORIENTED_EDGE('',*,*,#1188,.F.) ;
#1494 = ORIENTED_EDGE('',*,*,#1189,.T.) ;
#1495 = ORIENTED_EDGE('',*,*,#1190,.T.) ;
#1496 = ORIENTED_EDGE('',*,*,#1189,.F.) ;
#1497 = ORIENTED_EDGE('',*,*,#1191,.F.) ;
#1498 = ORIENTED_EDGE('',*,*,#1192,.F.) ;
#1499 = ORIENTED_EDGE('',*,*,#1193,.T.) ;
#1500 = ORIENTED_EDGE('',*,*,#1194,.T.) ;
#1501 = ORIENTED_EDGE('',*,*,#1195,.F.) ;
#1502 = ORIENTED_EDGE('',*,*,#1196,.F.) ;
#1503 = ORIENTED_EDGE('',*,*,#1197,.T.) ;
#1504 = ORIENTED_EDGE('',*,*,#1192,.T.) ;
#1505 = ORIENTED_EDGE('',*,*,#1198,.F.) ;
#1506 = ORIENTED_EDGE('',*,*,#1199,.F.) ;
#1507 = ORIENTED_EDGE('',*,*,#1200,.T.) ;
#1508 = ORIENTED_EDGE('',*,*,#1196,.T.) ;
#1509 = ORIENTED_EDGE('',*,*,#1201,.F.) ;
#1510 = ORIENTED_EDGE('',*,*,#1202,.F.) ;
#1511 = ORIENTED_EDGE('',*,*,#1203,.T.) ;
#1512 = ORIENTED_EDGE('',*,*,#1199,.T.) ;
#1513 = ORIENTED_EDGE('',*,*,#1204,.F.) ;
#1514 = ORIENTED_EDGE('',*,*,#1205,.F.) ;
#1515 = ORIENTED_EDGE('',*,*,#1206,.T.) ;
#1516 = ORIENTED_EDGE('',*,*,#1202,.T.) ;
#1517 = ORIENTED_EDGE('',*,*,#1207,.F.) ;
#1518 = ORIENTED_EDGE('',*,*,#1194,.F.) ;
#1519 = ORIENTED_EDGE('',*,*,#1208,.T.) ;
#1520 = ORIENTED_EDGE('',*,*,#1205,.T.) ;
#1521 = ORIENTED_EDGE('',*,*,#1193,.F.) ;
#1522 = ORIENTED_EDGE('',*,*,#1197,.F.) ;
#1523 = ORIENTED_EDGE('',*,*,#1200,.F.) ;
#1524 = ORIENTED_EDGE('',*,*,#1203,.F.) ;
#1525 = ORIENTED_EDGE('',*,*,#1206,.F.) ;
#1526 = ORIENTED_EDGE('',*,*,#1208,.F.) ;
#1527 = ORIENTED_EDGE('',*,*,#1140,.T.) ;
#1528 = ORIENTED_EDGE('',*,*,#1143,.T.) ;
#1529 = ORIENTED_EDGE('',*,*,#1146,.T.) ;
#1530 = ORIENTED_EDGE('',*,*,#1149,.T.) ;
#1531 = ORIENTED_EDGE('',*,*,#1152,.T.) ;
#1532 = ORIENTED_EDGE('',*,*,#1155,.T.) ;
#1533 = ORIENTED_EDGE('',*,*,#1158,.T.) ;
#1534 = ORIENTED_EDGE('',*,*,#1161,.T.) ;
#1535 = ORIENTED_EDGE('',*,*,#1164,.T.) ;
#1536 = ORIENTED_EDGE('',*,*,#1167,.T.) ;
#1537 = ORIENTED_EDGE('',*,*,#1170,.T.) ;
#1538 = ORIENTED_EDGE('',*,*,#1173,.T.) ;
#1539 = ORIENTED_EDGE('',*,*,#1176,.T.) ;
#1540 = ORIENTED_EDGE('',*,*,#1179,.T.) ;
#1541 = ORIENTED_EDGE('',*,*,#1182,.T.) ;
#1542 = ORIENTED_EDGE('',*,*,#1185,.T.) ;
#1543 = ORIENTED_EDGE('',*,*,#1188,.T.) ;
#1544 = ORIENTED_EDGE('',*,*,#1191,.T.) ;
#1545 = ORIENTED_EDGE('',*,*,#1207,.T.) ;
#1546 = ORIENTED_EDGE('',*,*,#1204,.T.) ;
#1547 = ORIENTED_EDGE('',*,*,#1201,.T.) ;
#1548 = ORIENTED_EDGE('',*,*,#1198,.T.) ;
#1549 = ORIENTED_EDGE('',*,*,#1195,.T.) ;
#1550 = ORIENTED_EDGE('',*,*,#1142,.F.) ;
#1551 = ORIENTED_EDGE('',*,*,#1145,.F.) ;
#1552 = ORIENTED_EDGE('',*,*,#1148,.F.) ;
#1553 = ORIENTED_EDGE('',*,*,#1151,.F.) ;
#1554 = ORIENTED_EDGE('',*,*,#1154,.F.) ;
#1555 = ORIENTED_EDGE('',*,*,#1157,.F.) ;
#1556 = ORIENTED_EDGE('',*,*,#1160,.F.) ;
#1557 = ORIENTED_EDGE('',*,*,#1163,.F.) ;
#1558 = ORIENTED_EDGE('',*,*,#1166,.F.) ;
#1559 = ORIENTED_EDGE('',*,*,#1169,.F.) ;
#1560 = ORIENTED_EDGE('',*,*,#1172,.F.) ;
#1561 = ORIENTED_EDGE('',*,*,#1175,.F.) ;
#1562 = ORIENTED_EDGE('',*,*,#1178,.F.) ;
#1563 = ORIENTED_EDGE('',*,*,#1181,.F.) ;
#1564 = ORIENTED_EDGE('',*,*,#1184,.F.) ;
#1565 = ORIENTED_EDGE('',*,*,#1187,.F.) ;
#1566 = ORIENTED_EDGE('',*,*,#1190,.F.) ;
#1567 = ORIENTED_EDGE('',*,*,#1209,.T.) ;
#1568 = ORIENTED_EDGE('',*,*,#1210,.T.) ;
#1569 = ORIENTED_EDGE('',*,*,#1211,.F.) ;
#1570 = ORIENTED_EDGE('',*,*,#1210,.F.) ;
#1571 = ORIENTED_EDGE('',*,*,#1212,.T.) ;
#1572 = ORIENTED_EDGE('',*,*,#1213,.T.) ;
#1573 = ORIENTED_EDGE('',*,*,#1214,.F.) ;
#1574 = ORIENTED_EDGE('',*,*,#1213,.F.) ;
#1575 = ORIENTED_EDGE('',*,*,#1215,.T.) ;
#1576 = ORIENTED_EDGE('',*,*,#1216,.T.) ;
#1577 = ORIENTED_EDGE('',*,*,#1217,.F.) ;
#1578 = ORIENTED_EDGE('',*,*,#1216,.F.) ;
#1579 = ORIENTED_EDGE('',*,*,#1218,.T.) ;
#1580 = ORIENTED_EDGE('',*,*,#1219,.T.) ;
#1581 = ORIENTED_EDGE('',*,*,#1220,.F.) ;
#1582 = ORIENTED_EDGE('',*,*,#1219,.F.) ;
#1583 = ORIENTED_EDGE('',*,*,#1221,.T.) ;
#1584 = ORIENTED_EDGE('',*,*,#1222,.T.) ;
#1585 = ORIENTED_EDGE('',*,*,#1223,.F.) ;
#1586 = ORIENTED_EDGE('',*,*,#1222,.F.) ;
#1587 = ORIENTED_EDGE('',*,*,#1224,.T.) ;
#1588 = ORIENTED_EDGE('',*,*,#1225,.T.) ;
#1589 = ORIENTED_EDGE('',*,*,#1226,.F.) ;
#1590 = ORIENTED_EDGE('',*,*,#1225,.F.) ;
#1591 = ORIENTED_EDGE('',*,*,#1227,.T.) ;
#1592 = ORIENTED_EDGE('',*,*,#1228,.T.) ;
#1593 = ORIENTED_EDGE('',*,*,#1229,.F.) ;
#1594 = ORIENTED_EDGE('',*,*,#1228,.F.) ;
#1595 = ORIENTED_EDGE('',*,*,#1230,.T.) ;
#1596 = ORIENTED_EDGE('',*,*,#1231,.T.) ;
#1597 = ORIENTED_EDGE('',*,*,#1232,.F.) ;
#1598 = ORIENTED_EDGE('',*,*,#1231,.F.) ;
#1599 = ORIENTED_EDGE('',*,*,#1233,.T.) ;
#1600 = ORIENTED_EDGE('',*,*,#1234,.T.) ;
#1601 = ORIENTED_EDGE('',*,*,#1235,.F.) ;
#1602 = ORIENTED_EDGE('',*,*,#1234,.F.) ;
#1603 = ORIENTED_EDGE('',*,*,#1236,.T.) ;
#1604 = ORIENTED_EDGE('',*,*,#1237,.T.) ;
#1605 = ORIENTED_EDGE('',*,*,#1238,.F.) ;
#1606 = ORIENTED_EDGE('',*,*,#1237,.F.) ;
#1607 = ORIENTED_EDGE('',*,*,#1239,.T.) ;
#1608 = ORIENTED_EDGE('',*,*,#1240,.T.) ;
#1609 = ORIENTED_EDGE('',*,*,#1241,.F.) ;
#1610 = ORIENTED_EDGE('',*,*,#1240,.F.) ;
#1611 = ORIENTED_EDGE('',*,*,#1242,.T.) ;
#1612 = ORIENTED_EDGE('',*,*,#1243,.T.) ;
#1613 = ORIENTED_EDGE('',*,*,#1244,.F.) ;
#1614 = ORIENTED_EDGE('',*,*,#1243,.F.) ;
#1615 = ORIENTED_EDGE('',*,*,#1245,.T.) ;
#1616 = ORIENTED_EDGE('',*,*,#1246,.T.) ;
#1617 = ORIENTED_EDGE('',*,*,#1247,.F.) ;
#1618 = ORIENTED_EDGE('',*,*,#1246,.F.) ;
#1619 = ORIENTED_EDGE('',*,*,#1248,.T.) ;
#1620 = ORIENTED_EDGE('',*,*,#1249,.T.) ;
#1621 = ORIENTED_EDGE('',*,*,#1250,.F.) ;
#1622 = ORIENTED_EDGE('',*,*,#1249,.F.) ;
#1623 = ORIENTED_EDGE('',*,*,#1251,.T.) ;
#1624 = ORIENTED_EDGE('',*,*,#1252,.T.) ;
#1625 = ORIENTED_EDGE('',*,*,#1253,.F.) ;
#1626 = ORIENTED_EDGE('',*,*,#1252,.F.) ;
#1627 = ORIENTED_EDGE('',*,*,#1254,.T.) ;
#1628 = ORIENTED_EDGE('',*,*,#1255,.T.) ;
#1629 = ORIENTED_EDGE('',*,*,#1256,.F.) ;
#1630 = ORIENTED_EDGE('',*,*,#1255,.F.) ;
#1631 = ORIENTED_EDGE('',*,*,#1257,.T.) ;
#1632 = ORIENTED_EDGE('',*,*,#1258,.T.) ;
#1633 = ORIENTED_EDGE('',*,*,#1259,.F.) ;
#1634 = ORIENTED_EDGE('',*,*,#1258,.F.) ;
#1635 = ORIENTED_EDGE('',*,*,#1260,.T.) ;
#1636 = ORIENTED_EDGE('',*,*,#1261,.T.) ;
#1637 = ORIENTED_EDGE('',*,*,#1262,.F.) ;
#1638 = ORIENTED_EDGE('',*,*,#1261,.F.) ;
#1639 = ORIENTED_EDGE('',*,*,#1263,.T.) ;
#1640 = ORIENTED_EDGE('',*,*,#1264,.T.) ;
#1641 = ORIENTED_EDGE('',*,*,#1265,.F.) ;
#1642 = ORIENTED_EDGE('',*,*,#1264,.F.) ;
#1643 = ORIENTED_EDGE('',*,*,#1266,.T.) ;
#1644 = ORIENTED_EDGE('',*,*,#1267,.T.) ;
#1645 = ORIENTED_EDGE('',*,*,#1268,.F.) ;
#1646 = ORIENTED_EDGE('',*,*,#1267,.F.) ;
#1647 = ORIENTED_EDGE('',*,*,#1269,.T.) ;
#1648 = ORIENTED_EDGE('',*,*,#1270,.T.) ;
#1649 = ORIENTED_EDGE('',*,*,#1271,.F.) ;
#1650 = ORIENTED_EDGE('',*,*,#1270,.F.) ;
#1651 = ORIENTED_EDGE('',*,*,#1272,.T.) ;
#1652 = ORIENTED_EDGE('',*,*,#1273,.T.) ;
#1653 = ORIENTED_EDGE('',*,*,#1274,.F.) ;
#1654 = ORIENTED_EDGE('',*,*,#1273,.F.) ;
#1655 = ORIENTED_EDGE('',*,*,#1275,.T.) ;
#1656 = ORIENTED_EDGE('',*,*,#1276,.T.) ;
#1657 = ORIENTED_EDGE('',*,*,#1277,.T.) ;
#1658 = ORIENTED_EDGE('',*,*,#1278,.T.) ;
#1659 = ORIENTED_EDGE('',*,*,#1279,.T.) ;
#1660 = ORIENTED_EDGE('',*,*,#1280,.T.) ;
#1661 = ORIENTED_EDGE('',*,*,#1281,.T.) ;
#1662 = ORIENTED_EDGE('',*,*,#1282,.T.) ;
#1663 = ORIENTED_EDGE('',*,*,#1283,.F.) ;
#1664 = ORIENTED_EDGE('',*,*,#1284,.F.) ;
#1665 = ORIENTED_EDGE('',*,*,#1285,.F.) ;
#1666 = ORIENTED_EDGE('',*,*,#1286,.F.) ;
#1667 = ORIENTED_EDGE('',*,*,#1269,.F.) ;
#1668 = ORIENTED_EDGE('',*,*,#1263,.F.) ;
#1669 = ORIENTED_EDGE('',*,*,#1257,.F.) ;
#1670 = ORIENTED_EDGE('',*,*,#1251,.F.) ;
#1671 = ORIENTED_EDGE('',*,*,#1245,.F.) ;
#1672 = ORIENTED_EDGE('',*,*,#1239,.F.) ;
#1673 = ORIENTED_EDGE('',*,*,#1233,.F.) ;
#1674 = ORIENTED_EDGE('',*,*,#1227,.F.) ;
#1675 = ORIENTED_EDGE('',*,*,#1221,.F.) ;
#1676 = ORIENTED_EDGE('',*,*,#1215,.F.) ;
#1677 = ORIENTED_EDGE('',*,*,#1209,.F.) ;
#1678 = ORIENTED_EDGE('',*,*,#1212,.F.) ;
#1679 = ORIENTED_EDGE('',*,*,#1218,.F.) ;
#1680 = ORIENTED_EDGE('',*,*,#1224,.F.) ;
#1681 = ORIENTED_EDGE('',*,*,#1230,.F.) ;
#1682 = ORIENTED_EDGE('',*,*,#1236,.F.) ;
#1683 = ORIENTED_EDGE('',*,*,#1242,.F.) ;
#1684 = ORIENTED_EDGE('',*,*,#1248,.F.) ;
#1685 = ORIENTED_EDGE('',*,*,#1254,.F.) ;
#1686 = ORIENTED_EDGE('',*,*,#1260,.F.) ;
#1687 = ORIENTED_EDGE('',*,*,#1266,.F.) ;
#1688 = ORIENTED_EDGE('',*,*,#1272,.F.) ;
#1689 = ORIENTED_EDGE('',*,*,#1287,.F.) ;
#1690 = ORIENTED_EDGE('',*,*,#1288,.F.) ;
#1691 = ORIENTED_EDGE('',*,*,#1289,.F.) ;
#1692 = ORIENTED_EDGE('',*,*,#1290,.F.) ;
#1693 = ORIENTED_EDGE('',*,*,#1291,.F.) ;
#1694 = ORIENTED_EDGE('',*,*,#1292,.F.) ;
#1695 = ORIENTED_EDGE('',*,*,#1293,.F.) ;
#1696 = ORIENTED_EDGE('',*,*,#1294,.F.) ;
#1697 = ORIENTED_EDGE('',*,*,#1295,.T.) ;
#1698 = ORIENTED_EDGE('',*,*,#1296,.T.) ;
#1699 = ORIENTED_EDGE('',*,*,#1297,.T.) ;
#1700 = ORIENTED_EDGE('',*,*,#1298,.T.) ;
#1701 = ORIENTED_EDGE('',*,*,#1274,.T.) ;
#1702 = ORIENTED_EDGE('',*,*,#1271,.T.) ;
#1703 = ORIENTED_EDGE('',*,*,#1268,.T.) ;
#1704 = ORIENTED_EDGE('',*,*,#1265,.T.) ;
#1705 = ORIENTED_EDGE('',*,*,#1262,.T.) ;
#1706 = ORIENTED_EDGE('',*,*,#1259,.T.) ;
#1707 = ORIENTED_EDGE('',*,*,#1256,.T.) ;
#1708 = ORIENTED_EDGE('',*,*,#1253,.T.) ;
#1709 = ORIENTED_EDGE('',*,*,#1250,.T.) ;
#1710 = ORIENTED_EDGE('',*,*,#1247,.T.) ;
#1711 = ORIENTED_EDGE('',*,*,#1244,.T.) ;
#1712 = ORIENTED_EDGE('',*,*,#1241,.T.) ;
#1713 = ORIENTED_EDGE('',*,*,#1238,.T.) ;
#1714 = ORIENTED_EDGE('',*,*,#1235,.T.) ;
#1715 = ORIENTED_EDGE('',*,*,#1232,.T.) ;
#1716 = ORIENTED_EDGE('',*,*,#1229,.T.) ;
#1717 = ORIENTED_EDGE('',*,*,#1226,.T.) ;
#1718 = ORIENTED_EDGE('',*,*,#1223,.T.) ;
#1719 = ORIENTED_EDGE('',*,*,#1220,.T.) ;
#1720 = ORIENTED_EDGE('',*,*,#1217,.T.) ;
#1721 = ORIENTED_EDGE('',*,*,#1214,.T.) ;
#1722 = ORIENTED_EDGE('',*,*,#1211,.T.) ;
#1723 = ORIENTED_EDGE('',*,*,#1287,.T.) ;
#1724 = ORIENTED_EDGE('',*,*,#1299,.F.) ;
#1725 = ORIENTED_EDGE('',*,*,#1275,.F.) ;
#1726 = ORIENTED_EDGE('',*,*,#1300,.T.) ;
#1727 = ORIENTED_EDGE('',*,*,#1294,.T.) ;
#1728 = ORIENTED_EDGE('',*,*,#1301,.F.) ;
#1729 = ORIENTED_EDGE('',*,*,#1276,.F.) ;
#1730 = ORIENTED_EDGE('',*,*,#1299,.T.) ;
#1731 = ORIENTED_EDGE('',*,*,#1293,.T.) ;
#1732 = ORIENTED_EDGE('',*,*,#1302,.F.) ;
#1733 = ORIENTED_EDGE('',*,*,#1277,.F.) ;
#1734 = ORIENTED_EDGE('',*,*,#1301,.T.) ;
#1735 = ORIENTED_EDGE('',*,*,#1292,.T.) ;
#1736 = ORIENTED_EDGE('',*,*,#1303,.F.) ;
#1737 = ORIENTED_EDGE('',*,*,#1278,.F.) ;
#1738 = ORIENTED_EDGE('',*,*,#1302,.T.) ;
#1739 = ORIENTED_EDGE('',*,*,#1291,.T.) ;
#1740 = ORIENTED_EDGE('',*,*,#1304,.F.) ;
#1741 = ORIENTED_EDGE('',*,*,#1279,.F.) ;
#1742 = ORIENTED_EDGE('',*,*,#1303,.T.) ;
#1743 = ORIENTED_EDGE('',*,*,#1290,.T.) ;
#1744 = ORIENTED_EDGE('',*,*,#1305,.F.) ;
#1745 = ORIENTED_EDGE('',*,*,#1280,.F.) ;
#1746 = ORIENTED_EDGE('',*,*,#1304,.T.) ;
#1747 = ORIENTED_EDGE('',*,*,#1289,.T.) ;
#1748 = ORIENTED_EDGE('',*,*,#1306,.F.) ;
#1749 = ORIENTED_EDGE('',*,*,#1281,.F.) ;
#1750 = ORIENTED_EDGE('',*,*,#1305,.T.) ;
#1751 = ORIENTED_EDGE('',*,*,#1288,.T.) ;
#1752 = ORIENTED_EDGE('',*,*,#1300,.F.) ;
#1753 = ORIENTED_EDGE('',*,*,#1282,.F.) ;
#1754 = ORIENTED_EDGE('',*,*,#1306,.T.) ;
#1755 = ORIENTED_EDGE('',*,*,#1295,.F.) ;
#1756 = ORIENTED_EDGE('',*,*,#1307,.F.) ;
#1757 = ORIENTED_EDGE('',*,*,#1284,.T.) ;
#1758 = ORIENTED_EDGE('',*,*,#1308,.T.) ;
#1759 = ORIENTED_EDGE('',*,*,#1296,.F.) ;
#1760 = ORIENTED_EDGE('',*,*,#1308,.F.) ;
#1761 = ORIENTED_EDGE('',*,*,#1283,.T.) ;
#1762 = ORIENTED_EDGE('',*,*,#1309,.T.) ;
#1763 = ORIENTED_EDGE('',*,*,#1297,.F.) ;
#1764 = ORIENTED_EDGE('',*,*,#1309,.F.) ;
#1765 = ORIENTED_EDGE('',*,*,#1286,.T.) ;
#1766 = ORIENTED_EDGE('',*,*,#1310,.T.) ;
#1767 = ORIENTED_EDGE('',*,*,#1298,.F.) ;
#1768 = ORIENTED_EDGE('',*,*,#1310,.F.) ;
#1769 = ORIENTED_EDGE('',*,*,#1285,.T.) ;
#1770 = ORIENTED_EDGE('',*,*,#1307,.T.) ;
#1771 = ORIENTED_EDGE('',*,*,#1311,.T.) ;
#1772 = ORIENTED_EDGE('',*,*,#1312,.F.) ;
#1773 = ORIENTED_EDGE('',*,*,#1313,.F.) ;
#1774 = ORIENTED_EDGE('',*,*,#1314,.T.) ;
#1775 = ORIENTED_EDGE('',*,*,#1315,.F.) ;
#1776 = ORIENTED_EDGE('',*,*,#1316,.F.) ;
#1777 = ORIENTED_EDGE('',*,*,#1317,.T.) ;
#1778 = ORIENTED_EDGE('',*,*,#1312,.T.) ;
#1779 = ORIENTED_EDGE('',*,*,#1318,.F.) ;
#1780 = ORIENTED_EDGE('',*,*,#1319,.F.) ;
#1781 = ORIENTED_EDGE('',*,*,#1320,.T.) ;
#1782 = ORIENTED_EDGE('',*,*,#1316,.T.) ;
#1783 = ORIENTED_EDGE('',*,*,#1321,.F.) ;
#1784 = ORIENTED_EDGE('',*,*,#1314,.F.) ;
#1785 = ORIENTED_EDGE('',*,*,#1322,.T.) ;
#1786 = ORIENTED_EDGE('',*,*,#1319,.T.) ;
#1787 = ORIENTED_EDGE('',*,*,#1313,.T.) ;
#1788 = ORIENTED_EDGE('',*,*,#1317,.F.) ;
#1789 = ORIENTED_EDGE('',*,*,#1320,.F.) ;
#1790 = ORIENTED_EDGE('',*,*,#1322,.F.) ;
#1791 = ORIENTED_EDGE('',*,*,#1311,.F.) ;
#1792 = ORIENTED_EDGE('',*,*,#1321,.T.) ;
#1793 = ORIENTED_EDGE('',*,*,#1318,.T.) ;
#1794 = ORIENTED_EDGE('',*,*,#1315,.T.) ;
#1795 = ORIENTED_EDGE('',*,*,#1323,.F.) ;
#1796 = ORIENTED_EDGE('',*,*,#1324,.F.) ;
#1797 = ORIENTED_EDGE('',*,*,#1325,.T.) ;
#1798 = ORIENTED_EDGE('',*,*,#1326,.T.) ;
#1799 = ORIENTED_EDGE('',*,*,#1327,.F.) ;
#1800 = ORIENTED_EDGE('',*,*,#1328,.F.) ;
#1801 = ORIENTED_EDGE('',*,*,#1329,.T.) ;
#1802 = ORIENTED_EDGE('',*,*,#1324,.T.) ;
#1803 = ORIENTED_EDGE('',*,*,#1330,.F.) ;
#1804 = ORIENTED_EDGE('',*,*,#1331,.F.) ;
#1805 = ORIENTED_EDGE('',*,*,#1332,.T.) ;
#1806 = ORIENTED_EDGE('',*,*,#1328,.T.) ;
#1807 = ORIENTED_EDGE('',*,*,#1333,.T.) ;
#1808 = ORIENTED_EDGE('',*,*,#1326,.F.) ;
#1809 = ORIENTED_EDGE('',*,*,#1334,.F.) ;
#1810 = ORIENTED_EDGE('',*,*,#1331,.T.) ;
#1811 = ORIENTED_EDGE('',*,*,#1334,.T.) ;
#1812 = ORIENTED_EDGE('',*,*,#1325,.F.) ;
#1813 = ORIENTED_EDGE('',*,*,#1329,.F.) ;
#1814 = ORIENTED_EDGE('',*,*,#1332,.F.) ;
#1815 = ORIENTED_EDGE('',*,*,#1323,.T.) ;
#1816 = ORIENTED_EDGE('',*,*,#1333,.F.) ;
#1817 = ORIENTED_EDGE('',*,*,#1330,.T.) ;
#1818 = ORIENTED_EDGE('',*,*,#1327,.T.) ;
#1819 = ORIENTED_EDGE('',*,*,#1335,.F.) ;
#1820 = ORIENTED_EDGE('',*,*,#1336,.F.) ;
#1821 = ORIENTED_EDGE('',*,*,#1337,.T.) ;
#1822 = ORIENTED_EDGE('',*,*,#1338,.T.) ;
#1823 = ORIENTED_EDGE('',*,*,#1339,.F.) ;
#1824 = ORIENTED_EDGE('',*,*,#1340,.F.) ;
#1825 = ORIENTED_EDGE('',*,*,#1341,.T.) ;
#1826 = ORIENTED_EDGE('',*,*,#1336,.T.) ;
#1827 = ORIENTED_EDGE('',*,*,#1342,.F.) ;
#1828 = ORIENTED_EDGE('',*,*,#1343,.F.) ;
#1829 = ORIENTED_EDGE('',*,*,#1344,.T.) ;
#1830 = ORIENTED_EDGE('',*,*,#1340,.T.) ;
#1831 = ORIENTED_EDGE('',*,*,#1345,.F.) ;
#1832 = ORIENTED_EDGE('',*,*,#1338,.F.) ;
#1833 = ORIENTED_EDGE('',*,*,#1346,.T.) ;
#1834 = ORIENTED_EDGE('',*,*,#1343,.T.) ;
#1835 = ORIENTED_EDGE('',*,*,#1337,.F.) ;
#1836 = ORIENTED_EDGE('',*,*,#1341,.F.) ;
#1837 = ORIENTED_EDGE('',*,*,#1344,.F.) ;
#1838 = ORIENTED_EDGE('',*,*,#1346,.F.) ;
#1839 = ORIENTED_EDGE('',*,*,#1335,.T.) ;
#1840 = ORIENTED_EDGE('',*,*,#1345,.T.) ;
#1841 = ORIENTED_EDGE('',*,*,#1342,.T.) ;
#1842 = ORIENTED_EDGE('',*,*,#1339,.T.) ;
#1843 = ORIENTED_EDGE('',*,*,#1347,.F.) ;
#1844 = ORIENTED_EDGE('',*,*,#1348,.F.) ;
#1845 = ORIENTED_EDGE('',*,*,#1349,.F.) ;
#1846 = ORIENTED_EDGE('',*,*,#1350,.T.) ;
#1847 = ORIENTED_EDGE('',*,*,#1351,.F.) ;
#1848 = ORIENTED_EDGE('',*,*,#1347,.T.) ;
#1849 = ORIENTED_EDGE('',*,*,#1352,.T.) ;
#1850 = ORIENTED_EDGE('',*,*,#1353,.F.) ;
#1851 = ORIENTED_EDGE('',*,*,#1354,.F.) ;
#1852 = ORIENTED_EDGE('',*,*,#1355,.T.) ;
#1853 = ORIENTED_EDGE('',*,*,#1356,.F.) ;
#1854 = ORIENTED_EDGE('',*,*,#1357,.F.) ;
#1855 = ORIENTED_EDGE('',*,*,#1358,.T.) ;
#1856 = ORIENTED_EDGE('',*,*,#1354,.T.) ;
#1857 = ORIENTED_EDGE('',*,*,#1359,.F.) ;
#1858 = ORIENTED_EDGE('',*,*,#1360,.T.) ;
#1859 = ORIENTED_EDGE('',*,*,#1361,.T.) ;
#1860 = ORIENTED_EDGE('',*,*,#1362,.F.) ;
#1861 = ORIENTED_EDGE('',*,*,#1352,.F.) ;
#1862 = ORIENTED_EDGE('',*,*,#1363,.T.) ;
#1863 = ORIENTED_EDGE('',*,*,#1364,.F.) ;
#1864 = ORIENTED_EDGE('',*,*,#1365,.F.) ;
#1865 = ORIENTED_EDGE('',*,*,#1353,.T.) ;
#1866 = ORIENTED_EDGE('',*,*,#1362,.T.) ;
#1867 = ORIENTED_EDGE('',*,*,#1366,.F.) ;
#1868 = ORIENTED_EDGE('',*,*,#1367,.F.) ;
#1869 = ORIENTED_EDGE('',*,*,#1351,.T.) ;
#1870 = ORIENTED_EDGE('',*,*,#1365,.T.) ;
#1871 = ORIENTED_EDGE('',*,*,#1355,.F.) ;
#1872 = ORIENTED_EDGE('',*,*,#1368,.F.) ;
#1873 = ORIENTED_EDGE('',*,*,#1348,.T.) ;
#1874 = ORIENTED_EDGE('',*,*,#1367,.T.) ;
#1875 = ORIENTED_EDGE('',*,*,#1358,.F.) ;
#1876 = ORIENTED_EDGE('',*,*,#1369,.F.) ;
#1877 = ORIENTED_EDGE('',*,*,#1370,.T.) ;
#1878 = ORIENTED_EDGE('',*,*,#1368,.T.) ;
#1879 = ORIENTED_EDGE('',*,*,#1360,.F.) ;
#1880 = ORIENTED_EDGE('',*,*,#1371,.F.) ;
#1881 = ORIENTED_EDGE('',*,*,#1372,.T.) ;
#1882 = ORIENTED_EDGE('',*,*,#1369,.T.) ;
#1883 = ORIENTED_EDGE('',*,*,#1359,.T.) ;
#1884 = ORIENTED_EDGE('',*,*,#1373,.F.) ;
#1885 = ORIENTED_EDGE('',*,*,#1374,.F.) ;
#1886 = ORIENTED_EDGE('',*,*,#1371,.T.) ;
#1887 = ORIENTED_EDGE('',*,*,#1357,.T.) ;
#1888 = ORIENTED_EDGE('',*,*,#1363,.F.) ;
#1889 = ORIENTED_EDGE('',*,*,#1350,.F.) ;
#1890 = ORIENTED_EDGE('',*,*,#1373,.T.) ;
#1891 = ORIENTED_EDGE('',*,*,#1374,.T.) ;
#1892 = ORIENTED_EDGE('',*,*,#1349,.T.) ;
#1893 = ORIENTED_EDGE('',*,*,#1370,.F.) ;
#1894 = ORIENTED_EDGE('',*,*,#1372,.F.) ;
#1895 = ORIENTED_EDGE('',*,*,#1361,.F.) ;
#1896 = ORIENTED_EDGE('',*,*,#1356,.T.) ;
#1897 = ORIENTED_EDGE('',*,*,#1366,.T.) ;
#1898 = ORIENTED_EDGE('',*,*,#1364,.T.) ;
#1899 = ORIENTED_EDGE('',*,*,#1375,.T.) ;
#1900 = ORIENTED_EDGE('',*,*,#1376,.F.) ;
#1901 = ORIENTED_EDGE('',*,*,#1377,.F.) ;
#1902 = ORIENTED_EDGE('',*,*,#1378,.T.) ;
#1903 = ORIENTED_EDGE('',*,*,#1379,.F.) ;
#1904 = ORIENTED_EDGE('',*,*,#1380,.F.) ;
#1905 = ORIENTED_EDGE('',*,*,#1381,.T.) ;
#1906 = ORIENTED_EDGE('',*,*,#1376,.T.) ;
#1907 = ORIENTED_EDGE('',*,*,#1382,.F.) ;
#1908 = ORIENTED_EDGE('',*,*,#1383,.F.) ;
#1909 = ORIENTED_EDGE('',*,*,#1384,.T.) ;
#1910 = ORIENTED_EDGE('',*,*,#1380,.T.) ;
#1911 = ORIENTED_EDGE('',*,*,#1385,.F.) ;
#1912 = ORIENTED_EDGE('',*,*,#1378,.F.) ;
#1913 = ORIENTED_EDGE('',*,*,#1386,.T.) ;
#1914 = ORIENTED_EDGE('',*,*,#1383,.T.) ;
#1915 = ORIENTED_EDGE('',*,*,#1377,.T.) ;
#1916 = ORIENTED_EDGE('',*,*,#1381,.F.) ;
#1917 = ORIENTED_EDGE('',*,*,#1384,.F.) ;
#1918 = ORIENTED_EDGE('',*,*,#1386,.F.) ;
#1919 = ORIENTED_EDGE('',*,*,#1375,.F.) ;
#1920 = ORIENTED_EDGE('',*,*,#1385,.T.) ;
#1921 = ORIENTED_EDGE('',*,*,#1382,.T.) ;
#1922 = ORIENTED_EDGE('',*,*,#1379,.T.) ;
#1923 = CYLINDRICAL_SURFACE('',#2182,47.5) ;
#1924 = CYLINDRICAL_SURFACE('',#2189,790.) ;
#1925 = CYLINDRICAL_SURFACE('',#2192,465.) ;
#1926 = CYLINDRICAL_SURFACE('',#2198,6.50000000001752) ;
#1927 = CYLINDRICAL_SURFACE('',#2201,6.50000000000472) ;
#1928 = CYLINDRICAL_SURFACE('',#2204,6.50000000000422) ;
#1929 = CYLINDRICAL_SURFACE('',#2207,6.50000000000406) ;
#1930 = CYLINDRICAL_SURFACE('',#2210,6.50000000000367) ;
#1931 = CYLINDRICAL_SURFACE('',#2213,6.50000000000261) ;
#1932 = CYLINDRICAL_SURFACE('',#2216,6.50000000000162) ;
#1933 = CYLINDRICAL_SURFACE('',#2219,6.50000000000089) ;
#1934 = CYLINDRICAL_SURFACE('',#2222,6.50000000000024) ;
#1935 = CYLINDRICAL_SURFACE('',#2225,6.49999999999945) ;
#1936 = CYLINDRICAL_SURFACE('',#2228,6.49999999999912) ;
#1937 = CYLINDRICAL_SURFACE('',#2231,6.49999999999901) ;
#1938 = CYLINDRICAL_SURFACE('',#2234,6.49999999999912) ;
#1939 = CYLINDRICAL_SURFACE('',#2237,6.49999999999928) ;
#1940 = CYLINDRICAL_SURFACE('',#2240,6.4999999999921) ;
#1941 = CYLINDRICAL_SURFACE('',#2243,6.50000000000001) ;
#1942 = CYLINDRICAL_SURFACE('',#2246,285.) ;
#1943 = CYLINDRICAL_SURFACE('',#2253,790.) ;
#1944 = CYLINDRICAL_SURFACE('',#2256,465.) ;
#1945 = CYLINDRICAL_SURFACE('',#2262,5.50000000000002) ;
#1946 = CYLINDRICAL_SURFACE('',#2265,5.50000000000002) ;
#1947 = CYLINDRICAL_SURFACE('',#2268,5.50000000000001) ;
#1948 = CYLINDRICAL_SURFACE('',#2271,5.50000000000001) ;
#1949 = CYLINDRICAL_SURFACE('',#2274,5.50000000000001) ;
#1950 = CYLINDRICAL_SURFACE('',#2277,5.50000000000001) ;
#1951 = CYLINDRICAL_SURFACE('',#2280,5.50000000000001) ;
#1952 = CYLINDRICAL_SURFACE('',#2283,5.50000000000001) ;
#1953 = CYLINDRICAL_SURFACE('',#2286,5.50000000000002) ;
#1954 = CYLINDRICAL_SURFACE('',#2289,5.50000000000002) ;
#1955 = CYLINDRICAL_SURFACE('',#2292,5.49999999999999) ;
#1956 = CYLINDRICAL_SURFACE('',#2295,5.49999999999999) ;
#1957 = CYLINDRICAL_SURFACE('',#2298,5.49999999999999) ;
#1958 = CYLINDRICAL_SURFACE('',#2301,5.49999999999999) ;
#1959 = CYLINDRICAL_SURFACE('',#2304,5.49999999999999) ;
#1960 = CYLINDRICAL_SURFACE('',#2307,5.50000000000002) ;
#1961 = CYLINDRICAL_SURFACE('',#2310,5.50000000000001) ;
#1962 = CYLINDRICAL_SURFACE('',#2313,5.50000000000001) ;
#1963 = CYLINDRICAL_SURFACE('',#2316,5.50000000000001) ;
#1964 = CYLINDRICAL_SURFACE('',#2319,5.50000000000001) ;
#1965 = CYLINDRICAL_SURFACE('',#2322,5.50000000000001) ;
#1966 = CYLINDRICAL_SURFACE('',#2325,5.50000000000001) ;
#1967 = CYLINDRICAL_SURFACE('',#2343,780.2) ;
#1968 = CYLINDRICAL_SURFACE('',#2347,785.) ;
#1969 = CYLINDRICAL_SURFACE('',#2355,460.) ;
#1970 = CYLINDRICAL_SURFACE('',#2359,455.2) ;
#1971 = CYLINDRICAL_SURFACE('',#2383,26.) ;
#1972 = CYLINDRICAL_SURFACE('',#2387,21.2) ;
#1973 = CYLINDRICAL_SURFACE('',#2391,780.2) ;
#1974 = CYLINDRICAL_SURFACE('',#2395,785.) ;
#1975 = ADVANCED_FACE('',(#213),#1923,.F.) ;
#1976 = ADVANCED_FACE('',(#214),#157,.T.) ;
#1977 = ADVANCED_FACE('',(#215),#158,.T.) ;
#1978 = ADVANCED_FACE('',(#216),#159,.T.) ;
#1979 = ADVANCED_FACE('',(#217),#160,.T.) ;
#1980 = ADVANCED_FACE('',(#218),#1924,.T.) ;
#1981 = ADVANCED_FACE('',(#219),#1925,.T.) ;
#1982 = ADVANCED_FACE('',(#220,#75),#161,.T.) ;
#1983 = ADVANCED_FACE('',(#221,#76),#162,.F.) ;
#1984 = ADVANCED_FACE('',(#222),#1926,.F.) ;
#1985 = ADVANCED_FACE('',(#223),#1927,.F.) ;
#1986 = ADVANCED_FACE('',(#224),#1928,.F.) ;
#1987 = ADVANCED_FACE('',(#225),#1929,.F.) ;
#1988 = ADVANCED_FACE('',(#226),#1930,.F.) ;
#1989 = ADVANCED_FACE('',(#227),#1931,.F.) ;
#1990 = ADVANCED_FACE('',(#228),#1932,.F.) ;
#1991 = ADVANCED_FACE('',(#229),#1933,.F.) ;
#1992 = ADVANCED_FACE('',(#230),#1934,.F.) ;
#1993 = ADVANCED_FACE('',(#231),#1935,.F.) ;
#1994 = ADVANCED_FACE('',(#232),#1936,.F.) ;
#1995 = ADVANCED_FACE('',(#233),#1937,.F.) ;
#1996 = ADVANCED_FACE('',(#234),#1938,.F.) ;
#1997 = ADVANCED_FACE('',(#235),#1939,.F.) ;
#1998 = ADVANCED_FACE('',(#236),#1940,.F.) ;
#1999 = ADVANCED_FACE('',(#237),#1941,.F.) ;
#2000 = ADVANCED_FACE('',(#238),#1942,.F.) ;
#2001 = ADVANCED_FACE('',(#239),#163,.T.) ;
#2002 = ADVANCED_FACE('',(#240),#164,.T.) ;
#2003 = ADVANCED_FACE('',(#241),#165,.T.) ;
#2004 = ADVANCED_FACE('',(#242),#166,.T.) ;
#2005 = ADVANCED_FACE('',(#243),#1943,.T.) ;
#2006 = ADVANCED_FACE('',(#244),#1944,.T.) ;
#2007 = ADVANCED_FACE('',(#245,#77,#78,#79,#80,#81,#82,#83,#84,#85,#86,#87,
#88,#89,#90,#91,#92,#93),#167,.T.) ;
#2008 = ADVANCED_FACE('',(#246,#94,#95,#96,#97,#98,#99,#100,#101,#102,#103,
#104,#105,#106,#107,#108,#109,#110),#168,.F.) ;
#2009 = ADVANCED_FACE('',(#247),#1945,.F.) ;
#2010 = ADVANCED_FACE('',(#248),#1946,.F.) ;
#2011 = ADVANCED_FACE('',(#249),#1947,.F.) ;
#2012 = ADVANCED_FACE('',(#250),#1948,.F.) ;
#2013 = ADVANCED_FACE('',(#251),#1949,.F.) ;
#2014 = ADVANCED_FACE('',(#252),#1950,.F.) ;
#2015 = ADVANCED_FACE('',(#253),#1951,.F.) ;
#2016 = ADVANCED_FACE('',(#254),#1952,.F.) ;
#2017 = ADVANCED_FACE('',(#255),#1953,.F.) ;
#2018 = ADVANCED_FACE('',(#256),#1954,.F.) ;
#2019 = ADVANCED_FACE('',(#257),#1955,.F.) ;
#2020 = ADVANCED_FACE('',(#258),#1956,.F.) ;
#2021 = ADVANCED_FACE('',(#259),#1957,.F.) ;
#2022 = ADVANCED_FACE('',(#260),#1958,.F.) ;
#2023 = ADVANCED_FACE('',(#261),#1959,.F.) ;
#2024 = ADVANCED_FACE('',(#262),#1960,.F.) ;
#2025 = ADVANCED_FACE('',(#263),#1961,.F.) ;
#2026 = ADVANCED_FACE('',(#264),#1962,.F.) ;
#2027 = ADVANCED_FACE('',(#265),#1963,.F.) ;
#2028 = ADVANCED_FACE('',(#266),#1964,.F.) ;
#2029 = ADVANCED_FACE('',(#267),#1965,.F.) ;
#2030 = ADVANCED_FACE('',(#268),#1966,.F.) ;
#2031 = ADVANCED_FACE('',(#269,#111,#112,#113,#114,#115,#116,#117,#118,#119,
#120,#121,#122,#123,#124,#125,#126,#127,#128,#129,#130,#131,#132,#133),
#169,.T.) ;
#2032 = ADVANCED_FACE('',(#270,#134,#135,#136,#137,#138,#139,#140,#141,#142,
#143,#144,#145,#146,#147,#148,#149,#150,#151,#152,#153,#154,#155,#156),
#170,.F.) ;
#2033 = ADVANCED_FACE('',(#271),#171,.F.) ;
#2034 = ADVANCED_FACE('',(#272),#172,.F.) ;
#2035 = ADVANCED_FACE('',(#273),#173,.F.) ;
#2036 = ADVANCED_FACE('',(#274),#174,.F.) ;
#2037 = ADVANCED_FACE('',(#275),#175,.F.) ;
#2038 = ADVANCED_FACE('',(#276),#176,.F.) ;
#2039 = ADVANCED_FACE('',(#277),#177,.F.) ;
#2040 = ADVANCED_FACE('',(#278),#178,.F.) ;
#2041 = ADVANCED_FACE('',(#279),#179,.T.) ;
#2042 = ADVANCED_FACE('',(#280),#180,.T.) ;
#2043 = ADVANCED_FACE('',(#281),#181,.T.) ;
#2044 = ADVANCED_FACE('',(#282),#182,.T.) ;
#2045 = ADVANCED_FACE('',(#283),#1967,.F.) ;
#2046 = ADVANCED_FACE('',(#284),#183,.T.) ;
#2047 = ADVANCED_FACE('',(#285),#1968,.T.) ;
#2048 = ADVANCED_FACE('',(#286),#184,.T.) ;
#2049 = ADVANCED_FACE('',(#287),#185,.T.) ;
#2050 = ADVANCED_FACE('',(#288),#186,.F.) ;
#2051 = ADVANCED_FACE('',(#289),#187,.T.) ;
#2052 = ADVANCED_FACE('',(#290),#1969,.T.) ;
#2053 = ADVANCED_FACE('',(#291),#188,.T.) ;
#2054 = ADVANCED_FACE('',(#292),#1970,.F.) ;
#2055 = ADVANCED_FACE('',(#293),#189,.T.) ;
#2056 = ADVANCED_FACE('',(#294),#190,.F.) ;
#2057 = ADVANCED_FACE('',(#295),#191,.T.) ;
#2058 = ADVANCED_FACE('',(#296),#192,.T.) ;
#2059 = ADVANCED_FACE('',(#297),#193,.T.) ;
#2060 = ADVANCED_FACE('',(#298),#194,.T.) ;
#2061 = ADVANCED_FACE('',(#299),#195,.F.) ;
#2062 = ADVANCED_FACE('',(#300),#196,.T.) ;
#2063 = ADVANCED_FACE('',(#301),#197,.T.) ;
#2064 = ADVANCED_FACE('',(#302),#198,.T.) ;
#2065 = ADVANCED_FACE('',(#303),#199,.T.) ;
#2066 = ADVANCED_FACE('',(#304),#200,.T.) ;
#2067 = ADVANCED_FACE('',(#305),#201,.F.) ;
#2068 = ADVANCED_FACE('',(#306),#202,.T.) ;
#2069 = ADVANCED_FACE('',(#307),#203,.T.) ;
#2070 = ADVANCED_FACE('',(#308),#1971,.T.) ;
#2071 = ADVANCED_FACE('',(#309),#204,.T.) ;
#2072 = ADVANCED_FACE('',(#310),#205,.T.) ;
#2073 = ADVANCED_FACE('',(#311),#206,.F.) ;
#2074 = ADVANCED_FACE('',(#312),#1972,.F.) ;
#2075 = ADVANCED_FACE('',(#313),#207,.F.) ;
#2076 = ADVANCED_FACE('',(#314),#208,.T.) ;
#2077 = ADVANCED_FACE('',(#315),#1973,.F.) ;
#2078 = ADVANCED_FACE('',(#316),#209,.T.) ;
#2079 = ADVANCED_FACE('',(#317),#1974,.T.) ;
#2080 = ADVANCED_FACE('',(#318),#210,.T.) ;
#2081 = ADVANCED_FACE('',(#319),#211,.T.) ;
#2082 = ADVANCED_FACE('',(#320),#212,.F.) ;
#2083 = CLOSED_SHELL('',(#1975,#1976,#1977,#1978,#1979,#1980,#1981,#1982,
#1983)) ;
#2084 = CLOSED_SHELL('',(#1984,#1985,#1986,#1987,#1988,#1989,#1990,#1991,
#1992,#1993,#1994,#1995,#1996,#1997,#1998,#1999,#2000,#2001,#2002,#2003,
#2004,#2005,#2006,#2007,#2008)) ;
#2085 = CLOSED_SHELL('',(#2009,#2010,#2011,#2012,#2013,#2014,#2015,#2016,
#2017,#2018,#2019,#2020,#2021,#2022,#2023,#2024,#2025,#2026,#2027,#2028,
#2029,#2030,#2031,#2032,#2033,#2034,#2035,#2036,#2037,#2038,#2039,#2040,
#2041,#2042,#2043,#2044)) ;
#2086 = CLOSED_SHELL('',(#2045,#2046,#2047,#2048,#2049,#2050)) ;
#2087 = CLOSED_SHELL('',(#2051,#2052,#2053,#2054,#2055,#2056)) ;
#2088 = CLOSED_SHELL('',(#2057,#2058,#2059,#2060,#2061,#2062)) ;
#2089 = CLOSED_SHELL('',(#2063,#2064,#2065,#2066,#2067,#2068,#2069,#2070,
#2071,#2072,#2073,#2074,#2075,#2076)) ;
#2090 = CLOSED_SHELL('',(#2077,#2078,#2079,#2080,#2081,#2082)) ;
#2091 = DERIVED_UNIT_ELEMENT(#2107,1.) ;
#2092 = DERIVED_UNIT_ELEMENT(#3621,-3.) ;
#2093 = DERIVED_UNIT_ELEMENT(#2107,1.) ;
#2094 = DERIVED_UNIT_ELEMENT(#3621,-3.) ;
#2095 = DERIVED_UNIT_ELEMENT(#2107,1.) ;
#2096 = DERIVED_UNIT_ELEMENT(#3621,-3.) ;
#2097 = DERIVED_UNIT_ELEMENT(#2107,1.) ;
#2098 = DERIVED_UNIT_ELEMENT(#3621,-3.) ;
#2099 = DERIVED_UNIT_ELEMENT(#2107,1.) ;
#2100 = DERIVED_UNIT_ELEMENT(#3621,-3.) ;
#2101 = DERIVED_UNIT_ELEMENT(#2107,1.) ;
#2102 = DERIVED_UNIT_ELEMENT(#3621,-3.) ;
#2103 = DERIVED_UNIT_ELEMENT(#2107,1.) ;
#2104 = DERIVED_UNIT_ELEMENT(#3621,-3.) ;
#2105 = DERIVED_UNIT_ELEMENT(#2107,1.) ;
#2106 = DERIVED_UNIT_ELEMENT(#3621,-3.) ;
#2107 = (
MASS_UNIT()
NAMED_UNIT(*)
SI_UNIT(.KILO.,.GRAM.)
) ;
#2108 = DERIVED_UNIT((#2091,#2092)) ;
#2109 = DERIVED_UNIT((#2093,#2094)) ;
#2110 = DERIVED_UNIT((#2095,#2096)) ;
#2111 = DERIVED_UNIT((#2097,#2098)) ;
#2112 = DERIVED_UNIT((#2099,#2100)) ;
#2113 = DERIVED_UNIT((#2101,#2102)) ;
#2114 = DERIVED_UNIT((#2103,#2104)) ;
#2115 = DERIVED_UNIT((#2105,#2106)) ;
#2116 = MEASURE_REPRESENTATION_ITEM('density measure',
POSITIVE_RATIO_MEASURE(7850.),#2108) ;
#2117 = MEASURE_REPRESENTATION_ITEM('density measure',
POSITIVE_RATIO_MEASURE(7850.),#2109) ;
#2118 = MEASURE_REPRESENTATION_ITEM('density measure',
POSITIVE_RATIO_MEASURE(7850.),#2110) ;
#2119 = MEASURE_REPRESENTATION_ITEM('density measure',
POSITIVE_RATIO_MEASURE(7850.),#2111) ;
#2120 = MEASURE_REPRESENTATION_ITEM('density measure',
POSITIVE_RATIO_MEASURE(7850.),#2112) ;
#2121 = MEASURE_REPRESENTATION_ITEM('density measure',
POSITIVE_RATIO_MEASURE(7850.),#2113) ;
#2122 = MEASURE_REPRESENTATION_ITEM('density measure',
POSITIVE_RATIO_MEASURE(7850.),#2114) ;
#2123 = MEASURE_REPRESENTATION_ITEM('density measure',
POSITIVE_RATIO_MEASURE(7850.),#2115) ;
#2124 = PROPERTY_DEFINITION_REPRESENTATION(#2164,#2140) ;
#2125 = PROPERTY_DEFINITION_REPRESENTATION(#2165,#2141) ;
#2126 = PROPERTY_DEFINITION_REPRESENTATION(#2166,#2142) ;
#2127 = PROPERTY_DEFINITION_REPRESENTATION(#2167,#2143) ;
#2128 = PROPERTY_DEFINITION_REPRESENTATION(#2168,#2144) ;
#2129 = PROPERTY_DEFINITION_REPRESENTATION(#2169,#2145) ;
#2130 = PROPERTY_DEFINITION_REPRESENTATION(#2170,#2146) ;
#2131 = PROPERTY_DEFINITION_REPRESENTATION(#2171,#2147) ;
#2132 = PROPERTY_DEFINITION_REPRESENTATION(#2172,#2148) ;
#2133 = PROPERTY_DEFINITION_REPRESENTATION(#2173,#2149) ;
#2134 = PROPERTY_DEFINITION_REPRESENTATION(#2174,#2150) ;
#2135 = PROPERTY_DEFINITION_REPRESENTATION(#2175,#2151) ;
#2136 = PROPERTY_DEFINITION_REPRESENTATION(#2176,#2152) ;
#2137 = PROPERTY_DEFINITION_REPRESENTATION(#2177,#2153) ;
#2138 = PROPERTY_DEFINITION_REPRESENTATION(#2178,#2154) ;
#2139 = PROPERTY_DEFINITION_REPRESENTATION(#2179,#2155) ;
#2140 = REPRESENTATION('material name',(#2156),#3611) ;
#2141 = REPRESENTATION('density',(#2116),#3611) ;
#2142 = REPRESENTATION('material name',(#2157),#3612) ;
#2143 = REPRESENTATION('density',(#2117),#3612) ;
#2144 = REPRESENTATION('material name',(#2158),#3613) ;
#2145 = REPRESENTATION('density',(#2118),#3613) ;
#2146 = REPRESENTATION('material name',(#2159),#3614) ;
#2147 = REPRESENTATION('density',(#2119),#3614) ;
#2148 = REPRESENTATION('material name',(#2160),#3615) ;
#2149 = REPRESENTATION('density',(#2120),#3615) ;
#2150 = REPRESENTATION('material name',(#2161),#3616) ;
#2151 = REPRESENTATION('density',(#2121),#3616) ;
#2152 = REPRESENTATION('material name',(#2162),#3617) ;
#2153 = REPRESENTATION('density',(#2122),#3617) ;
#2154 = REPRESENTATION('material name',(#2163),#3618) ;
#2155 = REPRESENTATION('density',(#2123),#3618) ;
#2156 = DESCRIPTIVE_REPRESENTATION_ITEM('Steel','Steel') ;
#2157 = DESCRIPTIVE_REPRESENTATION_ITEM('Steel','Steel') ;
#2158 = DESCRIPTIVE_REPRESENTATION_ITEM('Steel','Steel') ;
#2159 = DESCRIPTIVE_REPRESENTATION_ITEM('Steel','Steel') ;
#2160 = DESCRIPTIVE_REPRESENTATION_ITEM('Steel','Steel') ;
#2161 = DESCRIPTIVE_REPRESENTATION_ITEM('Steel','Steel') ;
#2162 = DESCRIPTIVE_REPRESENTATION_ITEM('Steel','Steel') ;
#2163 = DESCRIPTIVE_REPRESENTATION_ITEM('Steel','Steel') ;
#2164 = PROPERTY_DEFINITION('material property','material name',#3661) ;
#2165 = PROPERTY_DEFINITION('material property','density of part',#3661) ;
#2166 = PROPERTY_DEFINITION('material property','material name',#3662) ;
#2167 = PROPERTY_DEFINITION('material property','density of part',#3662) ;
#2168 = PROPERTY_DEFINITION('material property','material name',#3663) ;
#2169 = PROPERTY_DEFINITION('material property','density of part',#3663) ;
#2170 = PROPERTY_DEFINITION('material property','material name',#3664) ;
#2171 = PROPERTY_DEFINITION('material property','density of part',#3664) ;
#2172 = PROPERTY_DEFINITION('material property','material name',#3665) ;
#2173 = PROPERTY_DEFINITION('material property','density of part',#3665) ;
#2174 = PROPERTY_DEFINITION('material property','material name',#3666) ;
#2175 = PROPERTY_DEFINITION('material property','density of part',#3666) ;
#2176 = PROPERTY_DEFINITION('material property','material name',#3667) ;
#2177 = PROPERTY_DEFINITION('material property','density of part',#3667) ;
#2178 = PROPERTY_DEFINITION('material property','material name',#3668) ;
#2179 = PROPERTY_DEFINITION('material property','density of part',#3668) ;
#2180 = AXIS2_PLACEMENT_3D('',#3031,#2409,#2410) ;
#2181 = AXIS2_PLACEMENT_3D('',#3032,#2411,#2412) ;
#2182 = AXIS2_PLACEMENT_3D('',#3033,#2413,#2414) ;
#2183 = AXIS2_PLACEMENT_3D('',#3035,#2415,#2416) ;
#2184 = AXIS2_PLACEMENT_3D('',#3038,#2418,#2419) ;
#2185 = AXIS2_PLACEMENT_3D('',#3039,#2420,#2421) ;
#2186 = AXIS2_PLACEMENT_3D('',#3048,#2426,#2427) ;
#2187 = AXIS2_PLACEMENT_3D('',#3054,#2431,#2432) ;
#2188 = AXIS2_PLACEMENT_3D('',#3060,#2436,#2437) ;
#2189 = AXIS2_PLACEMENT_3D('',#3066,#2441,#2442) ;
#2190 = AXIS2_PLACEMENT_3D('',#3068,#2443,#2444) ;
#2191 = AXIS2_PLACEMENT_3D('',#3071,#2446,#2447) ;
#2192 = AXIS2_PLACEMENT_3D('',#3072,#2448,#2449) ;
#2193 = AXIS2_PLACEMENT_3D('',#3073,#2450,#2451) ;
#2194 = AXIS2_PLACEMENT_3D('',#3074,#2452,#2453) ;
#2195 = AXIS2_PLACEMENT_3D('',#3075,#2454,#2455) ;
#2196 = AXIS2_PLACEMENT_3D('',#3076,#2456,#2457) ;
#2197 = AXIS2_PLACEMENT_3D('',#3077,#2458,#2459) ;
#2198 = AXIS2_PLACEMENT_3D('',#3078,#2460,#2461) ;
#2199 = AXIS2_PLACEMENT_3D('',#3080,#2462,#2463) ;
#2200 = AXIS2_PLACEMENT_3D('',#3083,#2465,#2466) ;
#2201 = AXIS2_PLACEMENT_3D('',#3084,#2467,#2468) ;
#2202 = AXIS2_PLACEMENT_3D('',#3086,#2469,#2470) ;
#2203 = AXIS2_PLACEMENT_3D('',#3089,#2472,#2473) ;
#2204 = AXIS2_PLACEMENT_3D('',#3090,#2474,#2475) ;
#2205 = AXIS2_PLACEMENT_3D('',#3092,#2476,#2477) ;
#2206 = AXIS2_PLACEMENT_3D('',#3095,#2479,#2480) ;
#2207 = AXIS2_PLACEMENT_3D('',#3096,#2481,#2482) ;
#2208 = AXIS2_PLACEMENT_3D('',#3098,#2483,#2484) ;
#2209 = AXIS2_PLACEMENT_3D('',#3101,#2486,#2487) ;
#2210 = AXIS2_PLACEMENT_3D('',#3102,#2488,#2489) ;
#2211 = AXIS2_PLACEMENT_3D('',#3104,#2490,#2491) ;
#2212 = AXIS2_PLACEMENT_3D('',#3107,#2493,#2494) ;
#2213 = AXIS2_PLACEMENT_3D('',#3108,#2495,#2496) ;
#2214 = AXIS2_PLACEMENT_3D('',#3110,#2497,#2498) ;
#2215 = AXIS2_PLACEMENT_3D('',#3113,#2500,#2501) ;
#2216 = AXIS2_PLACEMENT_3D('',#3114,#2502,#2503) ;
#2217 = AXIS2_PLACEMENT_3D('',#3116,#2504,#2505) ;
#2218 = AXIS2_PLACEMENT_3D('',#3119,#2507,#2508) ;
#2219 = AXIS2_PLACEMENT_3D('',#3120,#2509,#2510) ;
#2220 = AXIS2_PLACEMENT_3D('',#3122,#2511,#2512) ;
#2221 = AXIS2_PLACEMENT_3D('',#3125,#2514,#2515) ;
#2222 = AXIS2_PLACEMENT_3D('',#3126,#2516,#2517) ;
#2223 = AXIS2_PLACEMENT_3D('',#3128,#2518,#2519) ;
#2224 = AXIS2_PLACEMENT_3D('',#3131,#2521,#2522) ;
#2225 = AXIS2_PLACEMENT_3D('',#3132,#2523,#2524) ;
#2226 = AXIS2_PLACEMENT_3D('',#3134,#2525,#2526) ;
#2227 = AXIS2_PLACEMENT_3D('',#3137,#2528,#2529) ;
#2228 = AXIS2_PLACEMENT_3D('',#3138,#2530,#2531) ;
#2229 = AXIS2_PLACEMENT_3D('',#3140,#2532,#2533) ;
#2230 = AXIS2_PLACEMENT_3D('',#3143,#2535,#2536) ;
#2231 = AXIS2_PLACEMENT_3D('',#3144,#2537,#2538) ;
#2232 = AXIS2_PLACEMENT_3D('',#3146,#2539,#2540) ;
#2233 = AXIS2_PLACEMENT_3D('',#3149,#2542,#2543) ;
#2234 = AXIS2_PLACEMENT_3D('',#3150,#2544,#2545) ;
#2235 = AXIS2_PLACEMENT_3D('',#3152,#2546,#2547) ;
#2236 = AXIS2_PLACEMENT_3D('',#3155,#2549,#2550) ;
#2237 = AXIS2_PLACEMENT_3D('',#3156,#2551,#2552) ;
#2238 = AXIS2_PLACEMENT_3D('',#3158,#2553,#2554) ;
#2239 = AXIS2_PLACEMENT_3D('',#3161,#2556,#2557) ;
#2240 = AXIS2_PLACEMENT_3D('',#3162,#2558,#2559) ;
#2241 = AXIS2_PLACEMENT_3D('',#3164,#2560,#2561) ;
#2242 = AXIS2_PLACEMENT_3D('',#3167,#2563,#2564) ;
#2243 = AXIS2_PLACEMENT_3D('',#3168,#2565,#2566) ;
#2244 = AXIS2_PLACEMENT_3D('',#3170,#2567,#2568) ;
#2245 = AXIS2_PLACEMENT_3D('',#3173,#2570,#2571) ;
#2246 = AXIS2_PLACEMENT_3D('',#3174,#2572,#2573) ;
#2247 = AXIS2_PLACEMENT_3D('',#3176,#2574,#2575) ;
#2248 = AXIS2_PLACEMENT_3D('',#3179,#2577,#2578) ;
#2249 = AXIS2_PLACEMENT_3D('',#3180,#2579,#2580) ;
#2250 = AXIS2_PLACEMENT_3D('',#3189,#2585,#2586) ;
#2251 = AXIS2_PLACEMENT_3D('',#3195,#2590,#2591) ;
#2252 = AXIS2_PLACEMENT_3D('',#3201,#2595,#2596) ;
#2253 = AXIS2_PLACEMENT_3D('',#3207,#2600,#2601) ;
#2254 = AXIS2_PLACEMENT_3D('',#3209,#2602,#2603) ;
#2255 = AXIS2_PLACEMENT_3D('',#3212,#2605,#2606) ;
#2256 = AXIS2_PLACEMENT_3D('',#3213,#2607,#2608) ;
#2257 = AXIS2_PLACEMENT_3D('',#3214,#2609,#2610) ;
#2258 = AXIS2_PLACEMENT_3D('',#3215,#2611,#2612) ;
#2259 = AXIS2_PLACEMENT_3D('',#3216,#2613,#2614) ;
#2260 = AXIS2_PLACEMENT_3D('',#3217,#2615,#2616) ;
#2261 = AXIS2_PLACEMENT_3D('',#3218,#2617,#2618) ;
#2262 = AXIS2_PLACEMENT_3D('',#3219,#2619,#2620) ;
#2263 = AXIS2_PLACEMENT_3D('',#3221,#2621,#2622) ;
#2264 = AXIS2_PLACEMENT_3D('',#3224,#2624,#2625) ;
#2265 = AXIS2_PLACEMENT_3D('',#3225,#2626,#2627) ;
#2266 = AXIS2_PLACEMENT_3D('',#3227,#2628,#2629) ;
#2267 = AXIS2_PLACEMENT_3D('',#3230,#2631,#2632) ;
#2268 = AXIS2_PLACEMENT_3D('',#3231,#2633,#2634) ;
#2269 = AXIS2_PLACEMENT_3D('',#3233,#2635,#2636) ;
#2270 = AXIS2_PLACEMENT_3D('',#3236,#2638,#2639) ;
#2271 = AXIS2_PLACEMENT_3D('',#3237,#2640,#2641) ;
#2272 = AXIS2_PLACEMENT_3D('',#3239,#2642,#2643) ;
#2273 = AXIS2_PLACEMENT_3D('',#3242,#2645,#2646) ;
#2274 = AXIS2_PLACEMENT_3D('',#3243,#2647,#2648) ;
#2275 = AXIS2_PLACEMENT_3D('',#3245,#2649,#2650) ;
#2276 = AXIS2_PLACEMENT_3D('',#3248,#2652,#2653) ;
#2277 = AXIS2_PLACEMENT_3D('',#3249,#2654,#2655) ;
#2278 = AXIS2_PLACEMENT_3D('',#3251,#2656,#2657) ;
#2279 = AXIS2_PLACEMENT_3D('',#3254,#2659,#2660) ;
#2280 = AXIS2_PLACEMENT_3D('',#3255,#2661,#2662) ;
#2281 = AXIS2_PLACEMENT_3D('',#3257,#2663,#2664) ;
#2282 = AXIS2_PLACEMENT_3D('',#3260,#2666,#2667) ;
#2283 = AXIS2_PLACEMENT_3D('',#3261,#2668,#2669) ;
#2284 = AXIS2_PLACEMENT_3D('',#3263,#2670,#2671) ;
#2285 = AXIS2_PLACEMENT_3D('',#3266,#2673,#2674) ;
#2286 = AXIS2_PLACEMENT_3D('',#3267,#2675,#2676) ;
#2287 = AXIS2_PLACEMENT_3D('',#3269,#2677,#2678) ;
#2288 = AXIS2_PLACEMENT_3D('',#3272,#2680,#2681) ;
#2289 = AXIS2_PLACEMENT_3D('',#3273,#2682,#2683) ;
#2290 = AXIS2_PLACEMENT_3D('',#3275,#2684,#2685) ;
#2291 = AXIS2_PLACEMENT_3D('',#3278,#2687,#2688) ;
#2292 = AXIS2_PLACEMENT_3D('',#3279,#2689,#2690) ;
#2293 = AXIS2_PLACEMENT_3D('',#3281,#2691,#2692) ;
#2294 = AXIS2_PLACEMENT_3D('',#3284,#2694,#2695) ;
#2295 = AXIS2_PLACEMENT_3D('',#3285,#2696,#2697) ;
#2296 = AXIS2_PLACEMENT_3D('',#3287,#2698,#2699) ;
#2297 = AXIS2_PLACEMENT_3D('',#3290,#2701,#2702) ;
#2298 = AXIS2_PLACEMENT_3D('',#3291,#2703,#2704) ;
#2299 = AXIS2_PLACEMENT_3D('',#3293,#2705,#2706) ;
#2300 = AXIS2_PLACEMENT_3D('',#3296,#2708,#2709) ;
#2301 = AXIS2_PLACEMENT_3D('',#3297,#2710,#2711) ;
#2302 = AXIS2_PLACEMENT_3D('',#3299,#2712,#2713) ;
#2303 = AXIS2_PLACEMENT_3D('',#3302,#2715,#2716) ;
#2304 = AXIS2_PLACEMENT_3D('',#3303,#2717,#2718) ;
#2305 = AXIS2_PLACEMENT_3D('',#3305,#2719,#2720) ;
#2306 = AXIS2_PLACEMENT_3D('',#3308,#2722,#2723) ;
#2307 = AXIS2_PLACEMENT_3D('',#3309,#2724,#2725) ;
#2308 = AXIS2_PLACEMENT_3D('',#3311,#2726,#2727) ;
#2309 = AXIS2_PLACEMENT_3D('',#3314,#2729,#2730) ;
#2310 = AXIS2_PLACEMENT_3D('',#3315,#2731,#2732) ;
#2311 = AXIS2_PLACEMENT_3D('',#3317,#2733,#2734) ;
#2312 = AXIS2_PLACEMENT_3D('',#3320,#2736,#2737) ;
#2313 = AXIS2_PLACEMENT_3D('',#3321,#2738,#2739) ;
#2314 = AXIS2_PLACEMENT_3D('',#3323,#2740,#2741) ;
#2315 = AXIS2_PLACEMENT_3D('',#3326,#2743,#2744) ;
#2316 = AXIS2_PLACEMENT_3D('',#3327,#2745,#2746) ;
#2317 = AXIS2_PLACEMENT_3D('',#3329,#2747,#2748) ;
#2318 = AXIS2_PLACEMENT_3D('',#3332,#2750,#2751) ;
#2319 = AXIS2_PLACEMENT_3D('',#3333,#2752,#2753) ;
#2320 = AXIS2_PLACEMENT_3D('',#3335,#2754,#2755) ;
#2321 = AXIS2_PLACEMENT_3D('',#3338,#2757,#2758) ;
#2322 = AXIS2_PLACEMENT_3D('',#3339,#2759,#2760) ;
#2323 = AXIS2_PLACEMENT_3D('',#3341,#2761,#2762) ;
#2324 = AXIS2_PLACEMENT_3D('',#3344,#2764,#2765) ;
#2325 = AXIS2_PLACEMENT_3D('',#3345,#2766,#2767) ;
#2326 = AXIS2_PLACEMENT_3D('',#3347,#2768,#2769) ;
#2327 = AXIS2_PLACEMENT_3D('',#3350,#2771,#2772) ;
#2328 = AXIS2_PLACEMENT_3D('',#3351,#2773,#2774) ;
#2329 = AXIS2_PLACEMENT_3D('',#3376,#2787,#2788) ;
#2330 = AXIS2_PLACEMENT_3D('',#3401,#2801,#2802) ;
#2331 = AXIS2_PLACEMENT_3D('',#3404,#2805,#2806) ;
#2332 = AXIS2_PLACEMENT_3D('',#3406,#2808,#2809) ;
#2333 = AXIS2_PLACEMENT_3D('',#3408,#2811,#2812) ;
#2334 = AXIS2_PLACEMENT_3D('',#3410,#2814,#2815) ;
#2335 = AXIS2_PLACEMENT_3D('',#3412,#2817,#2818) ;
#2336 = AXIS2_PLACEMENT_3D('',#3414,#2820,#2821) ;
#2337 = AXIS2_PLACEMENT_3D('',#3416,#2823,#2824) ;
#2338 = AXIS2_PLACEMENT_3D('',#3417,#2825,#2826) ;
#2339 = AXIS2_PLACEMENT_3D('',#3420,#2829,#2830) ;
#2340 = AXIS2_PLACEMENT_3D('',#3422,#2832,#2833) ;
#2341 = AXIS2_PLACEMENT_3D('',#3424,#2835,#2836) ;
#2342 = AXIS2_PLACEMENT_3D('',#3425,#2837,#2838) ;
#2343 = AXIS2_PLACEMENT_3D('',#3426,#2839,#2840) ;
#2344 = AXIS2_PLACEMENT_3D('',#3429,#2841,#2842) ;
#2345 = AXIS2_PLACEMENT_3D('',#3433,#2844,#2845) ;
#2346 = AXIS2_PLACEMENT_3D('',#3435,#2847,#2848) ;
#2347 = AXIS2_PLACEMENT_3D('',#3441,#2852,#2853) ;
#2348 = AXIS2_PLACEMENT_3D('',#3443,#2854,#2855) ;
#2349 = AXIS2_PLACEMENT_3D('',#3446,#2857,#2858) ;
#2350 = AXIS2_PLACEMENT_3D('',#3447,#2859,#2860) ;
#2351 = AXIS2_PLACEMENT_3D('',#3450,#2863,#2864) ;
#2352 = AXIS2_PLACEMENT_3D('',#3451,#2865,#2866) ;
#2353 = AXIS2_PLACEMENT_3D('',#3452,#2867,#2868) ;
#2354 = AXIS2_PLACEMENT_3D('',#3453,#2869,#2870) ;
#2355 = AXIS2_PLACEMENT_3D('',#3462,#2875,#2876) ;
#2356 = AXIS2_PLACEMENT_3D('',#3464,#2877,#2878) ;
#2357 = AXIS2_PLACEMENT_3D('',#3467,#2880,#2881) ;
#2358 = AXIS2_PLACEMENT_3D('',#3468,#2882,#2883) ;
#2359 = AXIS2_PLACEMENT_3D('',#3474,#2887,#2888) ;
#2360 = AXIS2_PLACEMENT_3D('',#3475,#2889,#2890) ;
#2361 = AXIS2_PLACEMENT_3D('',#3476,#2891,#2892) ;
#2362 = AXIS2_PLACEMENT_3D('',#3477,#2893,#2894) ;
#2363 = AXIS2_PLACEMENT_3D('',#3478,#2895,#2896) ;
#2364 = AXIS2_PLACEMENT_3D('',#3479,#2897,#2898) ;
#2365 = AXIS2_PLACEMENT_3D('',#3480,#2899,#2900) ;
#2366 = AXIS2_PLACEMENT_3D('',#3489,#2905,#2906) ;
#2367 = AXIS2_PLACEMENT_3D('',#3495,#2910,#2911) ;
#2368 = AXIS2_PLACEMENT_3D('',#3501,#2915,#2916) ;
#2369 = AXIS2_PLACEMENT_3D('',#3504,#2919,#2920) ;
#2370 = AXIS2_PLACEMENT_3D('',#3505,#2921,#2922) ;
#2371 = AXIS2_PLACEMENT_3D('',#3506,#2923,#2924) ;
#2372 = AXIS2_PLACEMENT_3D('',#3507,#2925,#2926) ;
#2373 = AXIS2_PLACEMENT_3D('',#3512,#2928,#2929) ;
#2374 = AXIS2_PLACEMENT_3D('',#3515,#2931,#2932) ;
#2375 = AXIS2_PLACEMENT_3D('',#3516,#2933,#2934) ;
#2376 = AXIS2_PLACEMENT_3D('',#3522,#2938,#2939) ;
#2377 = AXIS2_PLACEMENT_3D('',#3527,#2941,#2942) ;
#2378 = AXIS2_PLACEMENT_3D('',#3530,#2944,#2945) ;
#2379 = AXIS2_PLACEMENT_3D('',#3531,#2946,#2947) ;
#2380 = AXIS2_PLACEMENT_3D('',#3537,#2951,#2952) ;
#2381 = AXIS2_PLACEMENT_3D('',#3542,#2956,#2957) ;
#2382 = AXIS2_PLACEMENT_3D('',#3546,#2960,#2961) ;
#2383 = AXIS2_PLACEMENT_3D('',#3549,#2964,#2965) ;
#2384 = AXIS2_PLACEMENT_3D('',#3551,#2967,#2968) ;
#2385 = AXIS2_PLACEMENT_3D('',#3555,#2971,#2972) ;
#2386 = AXIS2_PLACEMENT_3D('',#3559,#2975,#2976) ;
#2387 = AXIS2_PLACEMENT_3D('',#3562,#2979,#2980) ;
#2388 = AXIS2_PLACEMENT_3D('',#3563,#2981,#2982) ;
#2389 = AXIS2_PLACEMENT_3D('',#3564,#2983,#2984) ;
#2390 = AXIS2_PLACEMENT_3D('',#3565,#2985,#2986) ;
#2391 = AXIS2_PLACEMENT_3D('',#3566,#2987,#2988) ;
#2392 = AXIS2_PLACEMENT_3D('',#3569,#2989,#2990) ;
#2393 = AXIS2_PLACEMENT_3D('',#3573,#2992,#2993) ;
#2394 = AXIS2_PLACEMENT_3D('',#3575,#2995,#2996) ;
#2395 = AXIS2_PLACEMENT_3D('',#3581,#3000,#3001) ;
#2396 = AXIS2_PLACEMENT_3D('',#3583,#3002,#3003) ;
#2397 = AXIS2_PLACEMENT_3D('',#3586,#3005,#3006) ;
#2398 = AXIS2_PLACEMENT_3D('',#3587,#3007,#3008) ;
#2399 = AXIS2_PLACEMENT_3D('',#3590,#3011,#3012) ;
#2400 = AXIS2_PLACEMENT_3D('',#3591,#3013,#3014) ;
#2401 = AXIS2_PLACEMENT_3D('',#3592,#3015,#3016) ;
#2402 = AXIS2_PLACEMENT_3D('',#3593,#3017,#3018) ;
#2403 = AXIS2_PLACEMENT_3D('',#3594,#3019,#3020) ;
#2404 = AXIS2_PLACEMENT_3D('',#3595,#3021,#3022) ;
#2405 = AXIS2_PLACEMENT_3D('',#3596,#3023,#3024) ;
#2406 = AXIS2_PLACEMENT_3D('',#3597,#3025,#3026) ;
#2407 = AXIS2_PLACEMENT_3D('',#3598,#3027,#3028) ;
#2408 = AXIS2_PLACEMENT_3D('',#3599,#3029,#3030) ;
#2409 = DIRECTION('axis',(0.,0.,1.)) ;
#2410 = DIRECTION('refdir',(1.,0.,0.)) ;
#2411 = DIRECTION('axis',(0.,0.,1.)) ;
#2412 = DIRECTION('refdir',(1.,0.,0.)) ;
#2413 = DIRECTION('center_axis',(0.,0.,1.)) ;
#2414 = DIRECTION('ref_axis',(1.,0.,0.)) ;
#2415 = DIRECTION('center_axis',(0.,0.,1.)) ;
#2416 = DIRECTION('ref_axis',(1.,0.,0.)) ;
#2417 = DIRECTION('',(0.,0.,1.)) ;
#2418 = DIRECTION('center_axis',(0.,0.,1.)) ;
#2419 = DIRECTION('ref_axis',(1.,0.,0.)) ;
#2420 = DIRECTION('center_axis',(1.81705896010664E-16,1.,0.)) ;
#2421 = DIRECTION('ref_axis',(-1.,1.81705896010664E-16,0.)) ;
#2422 = DIRECTION('',(-1.,1.81705896010664E-16,0.)) ;
#2423 = DIRECTION('',(0.,0.,1.)) ;
#2424 = DIRECTION('',(-1.,-2.46716227694479E-16,0.)) ;
#2425 = DIRECTION('',(0.,0.,1.)) ;
#2426 = DIRECTION('center_axis',(-1.,0.,0.)) ;
#2427 = DIRECTION('ref_axis',(0.,0.,1.)) ;
#2428 = DIRECTION('',(0.,-1.,0.)) ;
#2429 = DIRECTION('',(0.,0.,1.)) ;
#2430 = DIRECTION('',(0.,-1.,0.)) ;
#2431 = DIRECTION('center_axis',(-1.89944058960677E-16,1.,0.)) ;
#2432 = DIRECTION('ref_axis',(-1.,-1.89944058960677E-16,0.)) ;
#2433 = DIRECTION('',(-1.,-1.89944058960677E-16,0.)) ;
#2434 = DIRECTION('',(0.,0.,1.)) ;
#2435 = DIRECTION('',(-1.,-1.89944058960677E-16,0.)) ;
#2436 = DIRECTION('center_axis',(1.,0.,0.)) ;
#2437 = DIRECTION('ref_axis',(0.,0.,-1.)) ;
#2438 = DIRECTION('',(0.,1.,0.)) ;
#2439 = DIRECTION('',(0.,0.,1.)) ;
#2440 = DIRECTION('',(0.,1.,0.)) ;
#2441 = DIRECTION('center_axis',(0.,0.,1.)) ;
#2442 = DIRECTION('ref_axis',(1.,0.,0.)) ;
#2443 = DIRECTION('center_axis',(0.,0.,1.)) ;
#2444 = DIRECTION('ref_axis',(-1.,0.,0.)) ;
#2445 = DIRECTION('',(0.,0.,1.)) ;
#2446 = DIRECTION('center_axis',(0.,0.,1.)) ;
#2447 = DIRECTION('ref_axis',(-1.,0.,0.)) ;
#2448 = DIRECTION('center_axis',(0.,0.,1.)) ;
#2449 = DIRECTION('ref_axis',(1.,0.,0.)) ;
#2450 = DIRECTION('center_axis',(0.,0.,1.)) ;
#2451 = DIRECTION('ref_axis',(-1.,0.,0.)) ;
#2452 = DIRECTION('center_axis',(0.,0.,1.)) ;
#2453 = DIRECTION('ref_axis',(-1.,0.,0.)) ;
#2454 = DIRECTION('center_axis',(0.,0.,-1.)) ;
#2455 = DIRECTION('ref_axis',(-1.,0.,0.)) ;
#2456 = DIRECTION('center_axis',(0.,0.,-1.)) ;
#2457 = DIRECTION('ref_axis',(-1.,0.,0.)) ;
#2458 = DIRECTION('axis',(0.,0.,1.)) ;
#2459 = DIRECTION('refdir',(1.,0.,0.)) ;
#2460 = DIRECTION('center_axis',(0.,0.,1.)) ;
#2461 = DIRECTION('ref_axis',(1.,0.,0.)) ;
#2462 = DIRECTION('center_axis',(0.,0.,1.)) ;
#2463 = DIRECTION('ref_axis',(1.,0.,0.)) ;
#2464 = DIRECTION('',(0.,0.,1.)) ;
#2465 = DIRECTION('center_axis',(0.,0.,1.)) ;
#2466 = DIRECTION('ref_axis',(1.,0.,0.)) ;
#2467 = DIRECTION('center_axis',(0.,0.,1.)) ;
#2468 = DIRECTION('ref_axis',(1.,0.,0.)) ;
#2469 = DIRECTION('center_axis',(0.,0.,1.)) ;
#2470 = DIRECTION('ref_axis',(1.,0.,0.)) ;
#2471 = DIRECTION('',(0.,0.,1.)) ;
#2472 = DIRECTION('center_axis',(0.,0.,1.)) ;
#2473 = DIRECTION('ref_axis',(1.,0.,0.)) ;
#2474 = DIRECTION('center_axis',(0.,0.,1.)) ;
#2475 = DIRECTION('ref_axis',(1.,0.,0.)) ;
#2476 = DIRECTION('center_axis',(0.,0.,1.)) ;
#2477 = DIRECTION('ref_axis',(1.,0.,0.)) ;
#2478 = DIRECTION('',(0.,0.,1.)) ;
#2479 = DIRECTION('center_axis',(0.,0.,1.)) ;
#2480 = DIRECTION('ref_axis',(1.,0.,0.)) ;
#2481 = DIRECTION('center_axis',(0.,0.,1.)) ;
#2482 = DIRECTION('ref_axis',(1.,0.,0.)) ;
#2483 = DIRECTION('center_axis',(0.,0.,1.)) ;
#2484 = DIRECTION('ref_axis',(1.,0.,0.)) ;
#2485 = DIRECTION('',(0.,0.,1.)) ;
#2486 = DIRECTION('center_axis',(0.,0.,1.)) ;
#2487 = DIRECTION('ref_axis',(1.,0.,0.)) ;
#2488 = DIRECTION('center_axis',(0.,0.,1.)) ;
#2489 = DIRECTION('ref_axis',(1.,0.,0.)) ;
#2490 = DIRECTION('center_axis',(0.,0.,1.)) ;
#2491 = DIRECTION('ref_axis',(1.,0.,0.)) ;
#2492 = DIRECTION('',(0.,0.,1.)) ;
#2493 = DIRECTION('center_axis',(0.,0.,1.)) ;
#2494 = DIRECTION('ref_axis',(1.,0.,0.)) ;
#2495 = DIRECTION('center_axis',(0.,0.,1.)) ;
#2496 = DIRECTION('ref_axis',(1.,0.,0.)) ;
#2497 = DIRECTION('center_axis',(0.,0.,1.)) ;
#2498 = DIRECTION('ref_axis',(1.,0.,0.)) ;
#2499 = DIRECTION('',(0.,0.,1.)) ;
#2500 = DIRECTION('center_axis',(0.,0.,1.)) ;
#2501 = DIRECTION('ref_axis',(1.,0.,0.)) ;
#2502 = DIRECTION('center_axis',(0.,0.,1.)) ;
#2503 = DIRECTION('ref_axis',(1.,0.,0.)) ;
#2504 = DIRECTION('center_axis',(0.,0.,1.)) ;
#2505 = DIRECTION('ref_axis',(1.,0.,0.)) ;
#2506 = DIRECTION('',(0.,0.,1.)) ;
#2507 = DIRECTION('center_axis',(0.,0.,1.)) ;
#2508 = DIRECTION('ref_axis',(1.,0.,0.)) ;
#2509 = DIRECTION('center_axis',(0.,0.,1.)) ;
#2510 = DIRECTION('ref_axis',(1.,0.,0.)) ;
#2511 = DIRECTION('center_axis',(0.,0.,1.)) ;
#2512 = DIRECTION('ref_axis',(1.,0.,0.)) ;
#2513 = DIRECTION('',(0.,0.,1.)) ;
#2514 = DIRECTION('center_axis',(0.,0.,1.)) ;
#2515 = DIRECTION('ref_axis',(1.,0.,0.)) ;
#2516 = DIRECTION('center_axis',(0.,0.,1.)) ;
#2517 = DIRECTION('ref_axis',(1.,0.,0.)) ;
#2518 = DIRECTION('center_axis',(0.,0.,1.)) ;
#2519 = DIRECTION('ref_axis',(1.,0.,0.)) ;
#2520 = DIRECTION('',(0.,0.,1.)) ;
#2521 = DIRECTION('center_axis',(0.,0.,1.)) ;
#2522 = DIRECTION('ref_axis',(1.,0.,0.)) ;
#2523 = DIRECTION('center_axis',(0.,0.,1.)) ;
#2524 = DIRECTION('ref_axis',(1.,0.,0.)) ;
#2525 = DIRECTION('center_axis',(0.,0.,1.)) ;
#2526 = DIRECTION('ref_axis',(1.,0.,0.)) ;
#2527 = DIRECTION('',(0.,0.,1.)) ;
#2528 = DIRECTION('center_axis',(0.,0.,1.)) ;
#2529 = DIRECTION('ref_axis',(1.,0.,0.)) ;
#2530 = DIRECTION('center_axis',(0.,0.,1.)) ;
#2531 = DIRECTION('ref_axis',(1.,0.,0.)) ;
#2532 = DIRECTION('center_axis',(0.,0.,1.)) ;
#2533 = DIRECTION('ref_axis',(1.,0.,0.)) ;
#2534 = DIRECTION('',(0.,0.,1.)) ;
#2535 = DIRECTION('center_axis',(0.,0.,1.)) ;
#2536 = DIRECTION('ref_axis',(1.,0.,0.)) ;
#2537 = DIRECTION('center_axis',(0.,0.,1.)) ;
#2538 = DIRECTION('ref_axis',(1.,0.,0.)) ;
#2539 = DIRECTION('center_axis',(0.,0.,1.)) ;
#2540 = DIRECTION('ref_axis',(1.,0.,0.)) ;
#2541 = DIRECTION('',(0.,0.,1.)) ;
#2542 = DIRECTION('center_axis',(0.,0.,1.)) ;
#2543 = DIRECTION('ref_axis',(1.,0.,0.)) ;
#2544 = DIRECTION('center_axis',(0.,0.,1.)) ;
#2545 = DIRECTION('ref_axis',(1.,0.,0.)) ;
#2546 = DIRECTION('center_axis',(0.,0.,1.)) ;
#2547 = DIRECTION('ref_axis',(1.,0.,0.)) ;
#2548 = DIRECTION('',(0.,0.,1.)) ;
#2549 = DIRECTION('center_axis',(0.,0.,1.)) ;
#2550 = DIRECTION('ref_axis',(1.,0.,0.)) ;
#2551 = DIRECTION('center_axis',(0.,0.,1.)) ;
#2552 = DIRECTION('ref_axis',(1.,0.,0.)) ;
#2553 = DIRECTION('center_axis',(0.,0.,1.)) ;
#2554 = DIRECTION('ref_axis',(1.,0.,0.)) ;
#2555 = DIRECTION('',(0.,0.,1.)) ;
#2556 = DIRECTION('center_axis',(0.,0.,1.)) ;
#2557 = DIRECTION('ref_axis',(1.,0.,0.)) ;
#2558 = DIRECTION('center_axis',(0.,0.,1.)) ;
#2559 = DIRECTION('ref_axis',(1.,0.,0.)) ;
#2560 = DIRECTION('center_axis',(0.,0.,1.)) ;
#2561 = DIRECTION('ref_axis',(1.,0.,0.)) ;
#2562 = DIRECTION('',(0.,0.,1.)) ;
#2563 = DIRECTION('center_axis',(0.,0.,1.)) ;
#2564 = DIRECTION('ref_axis',(1.,0.,0.)) ;
#2565 = DIRECTION('center_axis',(0.,0.,1.)) ;
#2566 = DIRECTION('ref_axis',(1.,0.,0.)) ;
#2567 = DIRECTION('center_axis',(0.,0.,1.)) ;
#2568 = DIRECTION('ref_axis',(1.,0.,0.)) ;
#2569 = DIRECTION('',(0.,0.,1.)) ;
#2570 = DIRECTION('center_axis',(0.,0.,1.)) ;
#2571 = DIRECTION('ref_axis',(1.,0.,0.)) ;
#2572 = DIRECTION('center_axis',(0.,0.,1.)) ;
#2573 = DIRECTION('ref_axis',(1.,0.,0.)) ;
#2574 = DIRECTION('center_axis',(0.,0.,1.)) ;
#2575 = DIRECTION('ref_axis',(1.,0.,0.)) ;
#2576 = DIRECTION('',(0.,0.,1.)) ;
#2577 = DIRECTION('center_axis',(0.,0.,1.)) ;
#2578 = DIRECTION('ref_axis',(1.,0.,0.)) ;
#2579 = DIRECTION('center_axis',(0.,1.,0.)) ;
#2580 = DIRECTION('ref_axis',(0.,0.,1.)) ;
#2581 = DIRECTION('',(-1.,0.,0.)) ;
#2582 = DIRECTION('',(0.,0.,1.)) ;
#2583 = DIRECTION('',(-1.,-2.46716227694479E-16,0.)) ;
#2584 = DIRECTION('',(0.,0.,1.)) ;
#2585 = DIRECTION('center_axis',(-1.,1.95921710227969E-15,0.)) ;
#2586 = DIRECTION('ref_axis',(-1.95921710227969E-15,-1.,0.)) ;
#2587 = DIRECTION('',(-1.95921710227969E-15,-1.,0.)) ;
#2588 = DIRECTION('',(0.,0.,1.)) ;
#2589 = DIRECTION('',(-1.95921710227969E-15,-1.,0.)) ;
#2590 = DIRECTION('center_axis',(0.,1.,0.)) ;
#2591 = DIRECTION('ref_axis',(0.,0.,1.)) ;
#2592 = DIRECTION('',(-1.,0.,0.)) ;
#2593 = DIRECTION('',(0.,0.,1.)) ;
#2594 = DIRECTION('',(-1.,0.,0.)) ;
#2595 = DIRECTION('center_axis',(1.,0.,0.)) ;
#2596 = DIRECTION('ref_axis',(0.,0.,-1.)) ;
#2597 = DIRECTION('',(0.,1.,0.)) ;
#2598 = DIRECTION('',(0.,0.,1.)) ;
#2599 = DIRECTION('',(0.,1.,0.)) ;
#2600 = DIRECTION('center_axis',(0.,0.,1.)) ;
#2601 = DIRECTION('ref_axis',(1.,0.,0.)) ;
#2602 = DIRECTION('center_axis',(0.,0.,1.)) ;
#2603 = DIRECTION('ref_axis',(-1.,0.,0.)) ;
#2604 = DIRECTION('',(0.,0.,1.)) ;
#2605 = DIRECTION('center_axis',(0.,0.,1.)) ;
#2606 = DIRECTION('ref_axis',(-1.,0.,0.)) ;
#2607 = DIRECTION('center_axis',(0.,0.,1.)) ;
#2608 = DIRECTION('ref_axis',(1.,0.,0.)) ;
#2609 = DIRECTION('center_axis',(0.,0.,1.)) ;
#2610 = DIRECTION('ref_axis',(-1.,0.,0.)) ;
#2611 = DIRECTION('center_axis',(0.,0.,1.)) ;
#2612 = DIRECTION('ref_axis',(-1.,0.,0.)) ;
#2613 = DIRECTION('center_axis',(0.,0.,-1.)) ;
#2614 = DIRECTION('ref_axis',(-1.,0.,0.)) ;
#2615 = DIRECTION('center_axis',(0.,0.,-1.)) ;
#2616 = DIRECTION('ref_axis',(-1.,0.,0.)) ;
#2617 = DIRECTION('axis',(0.,0.,1.)) ;
#2618 = DIRECTION('refdir',(1.,0.,0.)) ;
#2619 = DIRECTION('center_axis',(0.,-1.,0.)) ;
#2620 = DIRECTION('ref_axis',(0.,0.,-1.)) ;
#2621 = DIRECTION('center_axis',(0.,1.,0.)) ;
#2622 = DIRECTION('ref_axis',(0.,0.,-1.)) ;
#2623 = DIRECTION('',(0.,-1.,0.)) ;
#2624 = DIRECTION('center_axis',(0.,1.,0.)) ;
#2625 = DIRECTION('ref_axis',(0.,0.,-1.)) ;
#2626 = DIRECTION('center_axis',(0.,-1.,0.)) ;
#2627 = DIRECTION('ref_axis',(0.,0.,-1.)) ;
#2628 = DIRECTION('center_axis',(0.,1.,0.)) ;
#2629 = DIRECTION('ref_axis',(0.,0.,-1.)) ;
#2630 = DIRECTION('',(0.,-1.,0.)) ;
#2631 = DIRECTION('center_axis',(0.,1.,0.)) ;
#2632 = DIRECTION('ref_axis',(0.,0.,-1.)) ;
#2633 = DIRECTION('center_axis',(0.,-1.,0.)) ;
#2634 = DIRECTION('ref_axis',(0.,0.,-1.)) ;
#2635 = DIRECTION('center_axis',(0.,1.,0.)) ;
#2636 = DIRECTION('ref_axis',(0.,0.,-1.)) ;
#2637 = DIRECTION('',(0.,-1.,0.)) ;
#2638 = DIRECTION('center_axis',(0.,1.,0.)) ;
#2639 = DIRECTION('ref_axis',(0.,0.,-1.)) ;
#2640 = DIRECTION('center_axis',(0.,-1.,0.)) ;
#2641 = DIRECTION('ref_axis',(0.,0.,-1.)) ;
#2642 = DIRECTION('center_axis',(0.,1.,0.)) ;
#2643 = DIRECTION('ref_axis',(0.,0.,-1.)) ;
#2644 = DIRECTION('',(0.,-1.,0.)) ;
#2645 = DIRECTION('center_axis',(0.,1.,0.)) ;
#2646 = DIRECTION('ref_axis',(0.,0.,-1.)) ;
#2647 = DIRECTION('center_axis',(0.,-1.,0.)) ;
#2648 = DIRECTION('ref_axis',(0.,0.,-1.)) ;
#2649 = DIRECTION('center_axis',(0.,1.,0.)) ;
#2650 = DIRECTION('ref_axis',(0.,0.,-1.)) ;
#2651 = DIRECTION('',(0.,-1.,0.)) ;
#2652 = DIRECTION('center_axis',(0.,1.,0.)) ;
#2653 = DIRECTION('ref_axis',(0.,0.,-1.)) ;
#2654 = DIRECTION('center_axis',(0.,-1.,0.)) ;
#2655 = DIRECTION('ref_axis',(0.,0.,-1.)) ;
#2656 = DIRECTION('center_axis',(0.,1.,0.)) ;
#2657 = DIRECTION('ref_axis',(0.,0.,1.)) ;
#2658 = DIRECTION('',(0.,-1.,0.)) ;
#2659 = DIRECTION('center_axis',(0.,1.,0.)) ;
#2660 = DIRECTION('ref_axis',(0.,0.,1.)) ;
#2661 = DIRECTION('center_axis',(0.,-1.,0.)) ;
#2662 = DIRECTION('ref_axis',(0.,0.,-1.)) ;
#2663 = DIRECTION('center_axis',(0.,1.,0.)) ;
#2664 = DIRECTION('ref_axis',(0.,0.,1.)) ;
#2665 = DIRECTION('',(0.,-1.,0.)) ;
#2666 = DIRECTION('center_axis',(0.,1.,0.)) ;
#2667 = DIRECTION('ref_axis',(0.,0.,1.)) ;
#2668 = DIRECTION('center_axis',(0.,-1.,0.)) ;
#2669 = DIRECTION('ref_axis',(0.,0.,-1.)) ;
#2670 = DIRECTION('center_axis',(0.,1.,0.)) ;
#2671 = DIRECTION('ref_axis',(0.,0.,1.)) ;
#2672 = DIRECTION('',(0.,-1.,0.)) ;
#2673 = DIRECTION('center_axis',(0.,1.,0.)) ;
#2674 = DIRECTION('ref_axis',(0.,0.,1.)) ;
#2675 = DIRECTION('center_axis',(0.,-1.,0.)) ;
#2676 = DIRECTION('ref_axis',(0.,0.,-1.)) ;
#2677 = DIRECTION('center_axis',(0.,1.,0.)) ;
#2678 = DIRECTION('ref_axis',(0.,0.,1.)) ;
#2679 = DIRECTION('',(0.,-1.,0.)) ;
#2680 = DIRECTION('center_axis',(0.,1.,0.)) ;
#2681 = DIRECTION('ref_axis',(0.,0.,1.)) ;
#2682 = DIRECTION('center_axis',(0.,-1.,0.)) ;
#2683 = DIRECTION('ref_axis',(0.,0.,-1.)) ;
#2684 = DIRECTION('center_axis',(0.,1.,0.)) ;
#2685 = DIRECTION('ref_axis',(0.,0.,1.)) ;
#2686 = DIRECTION('',(0.,-1.,0.)) ;
#2687 = DIRECTION('center_axis',(0.,1.,0.)) ;
#2688 = DIRECTION('ref_axis',(0.,0.,1.)) ;
#2689 = DIRECTION('center_axis',(0.,-1.,0.)) ;
#2690 = DIRECTION('ref_axis',(0.,0.,-1.)) ;
#2691 = DIRECTION('center_axis',(0.,1.,0.)) ;
#2692 = DIRECTION('ref_axis',(0.,0.,-1.)) ;
#2693 = DIRECTION('',(0.,-1.,0.)) ;
#2694 = DIRECTION('center_axis',(0.,1.,0.)) ;
#2695 = DIRECTION('ref_axis',(0.,0.,-1.)) ;
#2696 = DIRECTION('center_axis',(0.,-1.,0.)) ;
#2697 = DIRECTION('ref_axis',(0.,0.,-1.)) ;
#2698 = DIRECTION('center_axis',(0.,1.,0.)) ;
#2699 = DIRECTION('ref_axis',(0.,0.,-1.)) ;
#2700 = DIRECTION('',(0.,-1.,0.)) ;
#2701 = DIRECTION('center_axis',(0.,1.,0.)) ;
#2702 = DIRECTION('ref_axis',(0.,0.,-1.)) ;
#2703 = DIRECTION('center_axis',(0.,-1.,0.)) ;
#2704 = DIRECTION('ref_axis',(0.,0.,-1.)) ;
#2705 = DIRECTION('center_axis',(0.,1.,0.)) ;
#2706 = DIRECTION('ref_axis',(0.,0.,-1.)) ;
#2707 = DIRECTION('',(0.,-1.,0.)) ;
#2708 = DIRECTION('center_axis',(0.,1.,0.)) ;
#2709 = DIRECTION('ref_axis',(0.,0.,-1.)) ;
#2710 = DIRECTION('center_axis',(0.,-1.,0.)) ;
#2711 = DIRECTION('ref_axis',(0.,0.,-1.)) ;
#2712 = DIRECTION('center_axis',(0.,1.,0.)) ;
#2713 = DIRECTION('ref_axis',(0.,0.,-1.)) ;
#2714 = DIRECTION('',(0.,-1.,0.)) ;
#2715 = DIRECTION('center_axis',(0.,1.,0.)) ;
#2716 = DIRECTION('ref_axis',(0.,0.,-1.)) ;
#2717 = DIRECTION('center_axis',(0.,-1.,0.)) ;
#2718 = DIRECTION('ref_axis',(0.,0.,-1.)) ;
#2719 = DIRECTION('center_axis',(0.,1.,0.)) ;
#2720 = DIRECTION('ref_axis',(0.,0.,-1.)) ;
#2721 = DIRECTION('',(0.,-1.,0.)) ;
#2722 = DIRECTION('center_axis',(0.,1.,0.)) ;
#2723 = DIRECTION('ref_axis',(0.,0.,-1.)) ;
#2724 = DIRECTION('center_axis',(0.,-1.,0.)) ;
#2725 = DIRECTION('ref_axis',(0.,0.,-1.)) ;
#2726 = DIRECTION('center_axis',(0.,1.,0.)) ;
#2727 = DIRECTION('ref_axis',(0.,0.,-1.)) ;
#2728 = DIRECTION('',(0.,-1.,0.)) ;
#2729 = DIRECTION('center_axis',(0.,1.,0.)) ;
#2730 = DIRECTION('ref_axis',(0.,0.,-1.)) ;
#2731 = DIRECTION('center_axis',(0.,-1.,0.)) ;
#2732 = DIRECTION('ref_axis',(0.,0.,-1.)) ;
#2733 = DIRECTION('center_axis',(0.,1.,0.)) ;
#2734 = DIRECTION('ref_axis',(0.,0.,1.)) ;
#2735 = DIRECTION('',(0.,-1.,0.)) ;
#2736 = DIRECTION('center_axis',(0.,1.,0.)) ;
#2737 = DIRECTION('ref_axis',(0.,0.,1.)) ;
#2738 = DIRECTION('center_axis',(0.,-1.,0.)) ;
#2739 = DIRECTION('ref_axis',(0.,0.,-1.)) ;
#2740 = DIRECTION('center_axis',(0.,1.,0.)) ;
#2741 = DIRECTION('ref_axis',(0.,0.,1.)) ;
#2742 = DIRECTION('',(0.,-1.,0.)) ;
#2743 = DIRECTION('center_axis',(0.,1.,0.)) ;
#2744 = DIRECTION('ref_axis',(0.,0.,1.)) ;
#2745 = DIRECTION('center_axis',(0.,-1.,0.)) ;
#2746 = DIRECTION('ref_axis',(0.,0.,-1.)) ;
#2747 = DIRECTION('center_axis',(0.,1.,0.)) ;
#2748 = DIRECTION('ref_axis',(0.,0.,1.)) ;
#2749 = DIRECTION('',(0.,-1.,0.)) ;
#2750 = DIRECTION('center_axis',(0.,1.,0.)) ;
#2751 = DIRECTION('ref_axis',(0.,0.,1.)) ;
#2752 = DIRECTION('center_axis',(0.,-1.,0.)) ;
#2753 = DIRECTION('ref_axis',(0.,0.,-1.)) ;
#2754 = DIRECTION('center_axis',(0.,1.,0.)) ;
#2755 = DIRECTION('ref_axis',(0.,0.,1.)) ;
#2756 = DIRECTION('',(0.,-1.,0.)) ;
#2757 = DIRECTION('center_axis',(0.,1.,0.)) ;
#2758 = DIRECTION('ref_axis',(0.,0.,1.)) ;
#2759 = DIRECTION('center_axis',(0.,-1.,0.)) ;
#2760 = DIRECTION('ref_axis',(0.,0.,-1.)) ;
#2761 = DIRECTION('center_axis',(0.,1.,0.)) ;
#2762 = DIRECTION('ref_axis',(0.,0.,1.)) ;
#2763 = DIRECTION('',(0.,-1.,0.)) ;
#2764 = DIRECTION('center_axis',(0.,1.,0.)) ;
#2765 = DIRECTION('ref_axis',(0.,0.,1.)) ;
#2766 = DIRECTION('center_axis',(0.,-1.,0.)) ;
#2767 = DIRECTION('ref_axis',(0.,0.,-1.)) ;
#2768 = DIRECTION('center_axis',(0.,1.,0.)) ;
#2769 = DIRECTION('ref_axis',(0.,0.,1.)) ;
#2770 = DIRECTION('',(0.,-1.,0.)) ;
#2771 = DIRECTION('center_axis',(0.,1.,0.)) ;
#2772 = DIRECTION('ref_axis',(0.,0.,1.)) ;
#2773 = DIRECTION('center_axis',(0.,1.,0.)) ;
#2774 = DIRECTION('ref_axis',(0.,0.,1.)) ;
#2775 = DIRECTION('',(0.,0.,1.)) ;
#2776 = DIRECTION('',(0.707106781186546,0.,0.707106781186549)) ;
#2777 = DIRECTION('',(1.,0.,0.)) ;
#2778 = DIRECTION('',(0.707106781186549,0.,-0.707106781186546)) ;
#2779 = DIRECTION('',(0.,0.,-1.)) ;
#2780 = DIRECTION('',(-0.707106781186549,0.,-0.707106781186546)) ;
#2781 = DIRECTION('',(-1.,0.,0.)) ;
#2782 = DIRECTION('',(-0.707106781186546,0.,0.707106781186549)) ;
#2783 = DIRECTION('',(-1.,0.,0.)) ;
#2784 = DIRECTION('',(-2.46716227694479E-16,0.,-1.)) ;
#2785 = DIRECTION('',(1.,0.,0.)) ;
#2786 = DIRECTION('',(1.2335811384724E-16,0.,1.)) ;
#2787 = DIRECTION('center_axis',(0.,1.,0.)) ;
#2788 = DIRECTION('ref_axis',(0.,0.,1.)) ;
#2789 = DIRECTION('',(0.,0.,1.)) ;
#2790 = DIRECTION('',(-0.707106781186546,0.,0.707106781186549)) ;
#2791 = DIRECTION('',(-1.,0.,0.)) ;
#2792 = DIRECTION('',(-0.707106781186549,0.,-0.707106781186546)) ;
#2793 = DIRECTION('',(0.,0.,-1.)) ;
#2794 = DIRECTION('',(0.707106781186549,0.,-0.707106781186546)) ;
#2795 = DIRECTION('',(1.,0.,0.)) ;
#2796 = DIRECTION('',(0.707106781186546,0.,0.707106781186549)) ;
#2797 = DIRECTION('',(-2.46716227694479E-16,0.,-1.)) ;
#2798 = DIRECTION('',(-1.,0.,0.)) ;
#2799 = DIRECTION('',(1.2335811384724E-16,0.,1.)) ;
#2800 = DIRECTION('',(1.,0.,0.)) ;
#2801 = DIRECTION('center_axis',(1.,0.,0.)) ;
#2802 = DIRECTION('ref_axis',(0.,0.,-1.)) ;
#2803 = DIRECTION('',(0.,-1.,0.)) ;
#2804 = DIRECTION('',(0.,-1.,0.)) ;
#2805 = DIRECTION('center_axis',(0.707106781186549,0.,-0.707106781186546)) ;
#2806 = DIRECTION('ref_axis',(-0.707106781186546,0.,-0.707106781186549)) ;
#2807 = DIRECTION('',(0.,-1.,0.)) ;
#2808 = DIRECTION('center_axis',(0.,0.,-1.)) ;
#2809 = DIRECTION('ref_axis',(-1.,0.,0.)) ;
#2810 = DIRECTION('',(0.,-1.,0.)) ;
#2811 = DIRECTION('center_axis',(-0.707106781186546,0.,-0.707106781186549)) ;
#2812 = DIRECTION('ref_axis',(-0.707106781186549,0.,0.707106781186546)) ;
#2813 = DIRECTION('',(0.,-1.,0.)) ;
#2814 = DIRECTION('center_axis',(-1.,0.,0.)) ;
#2815 = DIRECTION('ref_axis',(0.,0.,1.)) ;
#2816 = DIRECTION('',(0.,-1.,0.)) ;
#2817 = DIRECTION('center_axis',(-0.707106781186546,0.,0.707106781186549)) ;
#2818 = DIRECTION('ref_axis',(0.707106781186549,0.,0.707106781186546)) ;
#2819 = DIRECTION('',(0.,-1.,0.)) ;
#2820 = DIRECTION('center_axis',(0.,0.,1.)) ;
#2821 = DIRECTION('ref_axis',(1.,0.,0.)) ;
#2822 = DIRECTION('',(0.,-1.,0.)) ;
#2823 = DIRECTION('center_axis',(0.707106781186549,0.,0.707106781186546)) ;
#2824 = DIRECTION('ref_axis',(0.707106781186546,0.,-0.707106781186549)) ;
#2825 = DIRECTION('center_axis',(-1.,0.,2.46716227694479E-16)) ;
#2826 = DIRECTION('ref_axis',(2.46716227694479E-16,0.,1.)) ;
#2827 = DIRECTION('',(0.,-1.,0.)) ;
#2828 = DIRECTION('',(0.,-1.,0.)) ;
#2829 = DIRECTION('center_axis',(0.,0.,1.)) ;
#2830 = DIRECTION('ref_axis',(1.,0.,0.)) ;
#2831 = DIRECTION('',(0.,-1.,0.)) ;
#2832 = DIRECTION('center_axis',(1.,0.,-1.2335811384724E-16)) ;
#2833 = DIRECTION('ref_axis',(-1.2335811384724E-16,0.,-1.)) ;
#2834 = DIRECTION('',(0.,-1.,0.)) ;
#2835 = DIRECTION('center_axis',(0.,0.,-1.)) ;
#2836 = DIRECTION('ref_axis',(-1.,0.,0.)) ;
#2837 = DIRECTION('axis',(0.,0.,1.)) ;
#2838 = DIRECTION('refdir',(1.,0.,0.)) ;
#2839 = DIRECTION('center_axis',(0.,0.,-1.)) ;
#2840 = DIRECTION('ref_axis',(-1.,0.,0.)) ;
#2841 = DIRECTION('center_axis',(0.,0.,-1.)) ;
#2842 = DIRECTION('ref_axis',(1.,0.,0.)) ;
#2843 = DIRECTION('',(0.,0.,-1.)) ;
#2844 = DIRECTION('center_axis',(0.,0.,-1.)) ;
#2845 = DIRECTION('ref_axis',(1.,0.,0.)) ;
#2846 = DIRECTION('',(0.,0.,-1.)) ;
#2847 = DIRECTION('center_axis',(-1.,-5.99005365632946E-14,0.)) ;
#2848 = DIRECTION('ref_axis',(5.99005365632946E-14,-1.,0.)) ;
#2849 = DIRECTION('',(-5.99005365632946E-14,1.,0.)) ;
#2850 = DIRECTION('',(0.,0.,-1.)) ;
#2851 = DIRECTION('',(-5.99005365632946E-14,1.,0.)) ;
#2852 = DIRECTION('center_axis',(0.,0.,-1.)) ;
#2853 = DIRECTION('ref_axis',(-1.,0.,0.)) ;
#2854 = DIRECTION('center_axis',(0.,0.,-1.)) ;
#2855 = DIRECTION('ref_axis',(-1.,0.,0.)) ;
#2856 = DIRECTION('',(0.,0.,-1.)) ;
#2857 = DIRECTION('center_axis',(0.,0.,-1.)) ;
#2858 = DIRECTION('ref_axis',(-1.,0.,0.)) ;
#2859 = DIRECTION('center_axis',(-1.22464679914736E-16,1.,0.)) ;
#2860 = DIRECTION('ref_axis',(-1.,-1.22464679914736E-16,0.)) ;
#2861 = DIRECTION('',(1.,1.22464679914736E-16,0.)) ;
#2862 = DIRECTION('',(1.,1.22464679914736E-16,0.)) ;
#2863 = DIRECTION('center_axis',(0.,0.,1.)) ;
#2864 = DIRECTION('ref_axis',(1.,0.,0.)) ;
#2865 = DIRECTION('center_axis',(0.,0.,1.)) ;
#2866 = DIRECTION('ref_axis',(1.,0.,0.)) ;
#2867 = DIRECTION('axis',(0.,0.,1.)) ;
#2868 = DIRECTION('refdir',(1.,0.,0.)) ;
#2869 = DIRECTION('center_axis',(0.898794046299161,-0.438371146789089,0.)) ;
#2870 = DIRECTION('ref_axis',(0.438371146789089,0.898794046299161,0.)) ;
#2871 = DIRECTION('',(-0.438371146789089,-0.898794046299161,0.)) ;
#2872 = DIRECTION('',(0.,0.,-1.)) ;
#2873 = DIRECTION('',(-0.438371146789089,-0.898794046299161,0.)) ;
#2874 = DIRECTION('',(0.,0.,-1.)) ;
#2875 = DIRECTION('center_axis',(0.,0.,-1.)) ;
#2876 = DIRECTION('ref_axis',(-1.,0.,0.)) ;
#2877 = DIRECTION('center_axis',(0.,0.,-1.)) ;
#2878 = DIRECTION('ref_axis',(-1.,0.,0.)) ;
#2879 = DIRECTION('',(0.,0.,-1.)) ;
#2880 = DIRECTION('center_axis',(0.,0.,-1.)) ;
#2881 = DIRECTION('ref_axis',(-1.,0.,0.)) ;
#2882 = DIRECTION('center_axis',(1.1613733811914E-14,-1.,0.)) ;
#2883 = DIRECTION('ref_axis',(1.,1.1613733811914E-14,0.)) ;
#2884 = DIRECTION('',(-1.,-1.1613733811914E-14,0.)) ;
#2885 = DIRECTION('',(0.,0.,-1.)) ;
#2886 = DIRECTION('',(-1.,-1.1613733811914E-14,0.)) ;
#2887 = DIRECTION('center_axis',(0.,0.,-1.)) ;
#2888 = DIRECTION('ref_axis',(-1.,0.,0.)) ;
#2889 = DIRECTION('center_axis',(0.,0.,-1.)) ;
#2890 = DIRECTION('ref_axis',(1.,0.,0.)) ;
#2891 = DIRECTION('center_axis',(0.,0.,-1.)) ;
#2892 = DIRECTION('ref_axis',(1.,0.,0.)) ;
#2893 = DIRECTION('center_axis',(0.,0.,1.)) ;
#2894 = DIRECTION('ref_axis',(1.,0.,0.)) ;
#2895 = DIRECTION('center_axis',(0.,0.,1.)) ;
#2896 = DIRECTION('ref_axis',(1.,0.,0.)) ;
#2897 = DIRECTION('axis',(0.,0.,1.)) ;
#2898 = DIRECTION('refdir',(1.,0.,0.)) ;
#2899 = DIRECTION('center_axis',(3.11423403168202E-19,-2.44394566430984E-20,
1.)) ;
#2900 = DIRECTION('ref_axis',(1.,-1.80411241501588E-16,-3.11423403168202E-19)) ;
#2901 = DIRECTION('',(1.80411241501588E-16,1.,2.44394566430984E-20)) ;
#2902 = DIRECTION('',(-1.,1.80411241501588E-16,3.11423403168202E-19)) ;
#2903 = DIRECTION('',(1.80411241501588E-16,1.,2.44394566430984E-20)) ;
#2904 = DIRECTION('',(-1.,1.80411241501588E-16,3.11423403168202E-19)) ;
#2905 = DIRECTION('center_axis',(-1.80411241501588E-16,-1.,-2.44394566430983E-20)) ;
#2906 = DIRECTION('ref_axis',(1.,-1.80411241501588E-16,-3.11423403168202E-19)) ;
#2907 = DIRECTION('',(3.11423403168202E-19,-2.44394566430984E-20,1.)) ;
#2908 = DIRECTION('',(-1.,1.80411241501588E-16,3.11423403168202E-19)) ;
#2909 = DIRECTION('',(3.11423403168202E-19,-2.44394566430984E-20,1.)) ;
#2910 = DIRECTION('center_axis',(-3.11423403168238E-19,-2.01834292293385E-16,
-1.)) ;
#2911 = DIRECTION('ref_axis',(-1.80411241501588E-16,-1.,2.01834292293385E-16)) ;
#2912 = DIRECTION('',(-1.80411241501588E-16,-1.,2.01834292293385E-16)) ;
#2913 = DIRECTION('',(-1.,1.80411241501588E-16,3.11423403168202E-19)) ;
#2914 = DIRECTION('',(-1.80411241501588E-16,-1.,2.01834292293385E-16)) ;
#2915 = DIRECTION('center_axis',(1.80411241501588E-16,1.,2.44394566430983E-20)) ;
#2916 = DIRECTION('ref_axis',(-1.,1.80411241501588E-16,3.11423403168202E-19)) ;
#2917 = DIRECTION('',(-3.11423403168202E-19,2.44394566430984E-20,-1.)) ;
#2918 = DIRECTION('',(-3.11423403168202E-19,2.44394566430984E-20,-1.)) ;
#2919 = DIRECTION('center_axis',(-1.,1.80411241501588E-16,3.11423403168202E-19)) ;
#2920 = DIRECTION('ref_axis',(3.11423403168202E-19,-2.44394566430984E-20,
1.)) ;
#2921 = DIRECTION('center_axis',(-1.,1.80411241501588E-16,3.11423403168202E-19)) ;
#2922 = DIRECTION('ref_axis',(3.11423403168202E-19,-2.44394566430984E-20,
1.)) ;
#2923 = DIRECTION('axis',(0.,0.,1.)) ;
#2924 = DIRECTION('refdir',(1.,0.,0.)) ;
#2925 = DIRECTION('center_axis',(0.,0.,1.)) ;
#2926 = DIRECTION('ref_axis',(1.,0.,0.)) ;
#2927 = DIRECTION('',(0.,1.,0.)) ;
#2928 = DIRECTION('center_axis',(0.,0.,-1.)) ;
#2929 = DIRECTION('ref_axis',(-1.,0.,0.)) ;
#2930 = DIRECTION('',(1.,7.2280144832367E-15,0.)) ;
#2931 = DIRECTION('center_axis',(0.,0.,-1.)) ;
#2932 = DIRECTION('ref_axis',(1.,0.,0.)) ;
#2933 = DIRECTION('center_axis',(0.,0.,1.)) ;
#2934 = DIRECTION('ref_axis',(1.,0.,0.)) ;
#2935 = DIRECTION('',(-1.,-1.22464679914735E-16,0.)) ;
#2936 = DIRECTION('',(-1.,-1.22464679914735E-16,0.)) ;
#2937 = DIRECTION('',(0.,1.,0.)) ;
#2938 = DIRECTION('center_axis',(0.,0.,-1.)) ;
#2939 = DIRECTION('ref_axis',(-1.,0.,0.)) ;
#2940 = DIRECTION('',(-1.,-7.2280144832367E-15,0.)) ;
#2941 = DIRECTION('center_axis',(0.,0.,-1.)) ;
#2942 = DIRECTION('ref_axis',(-1.,0.,0.)) ;
#2943 = DIRECTION('',(0.,-1.,0.)) ;
#2944 = DIRECTION('center_axis',(0.,0.,-1.)) ;
#2945 = DIRECTION('ref_axis',(1.,0.,0.)) ;
#2946 = DIRECTION('center_axis',(0.,0.,-1.)) ;
#2947 = DIRECTION('ref_axis',(-1.,0.,0.)) ;
#2948 = DIRECTION('',(0.,-1.,0.)) ;
#2949 = DIRECTION('',(0.,-1.,0.)) ;
#2950 = DIRECTION('',(1.,0.,0.)) ;
#2951 = DIRECTION('center_axis',(1.22464679914735E-16,-1.,0.)) ;
#2952 = DIRECTION('ref_axis',(1.,1.22464679914735E-16,0.)) ;
#2953 = DIRECTION('',(-1.,-1.22464679914735E-16,0.)) ;
#2954 = DIRECTION('',(0.,0.,-1.)) ;
#2955 = DIRECTION('',(0.,0.,-1.)) ;
#2956 = DIRECTION('center_axis',(-1.,0.,0.)) ;
#2957 = DIRECTION('ref_axis',(0.,0.,1.)) ;
#2958 = DIRECTION('',(0.,1.,0.)) ;
#2959 = DIRECTION('',(0.,0.,-1.)) ;
#2960 = DIRECTION('center_axis',(1.22464679914735E-16,-1.,0.)) ;
#2961 = DIRECTION('ref_axis',(1.,1.22464679914735E-16,0.)) ;
#2962 = DIRECTION('',(-1.,-1.22464679914735E-16,0.)) ;
#2963 = DIRECTION('',(0.,0.,-1.)) ;
#2964 = DIRECTION('center_axis',(0.,0.,-1.)) ;
#2965 = DIRECTION('ref_axis',(-1.,0.,0.)) ;
#2966 = DIRECTION('',(0.,0.,-1.)) ;
#2967 = DIRECTION('center_axis',(1.,0.,0.)) ;
#2968 = DIRECTION('ref_axis',(0.,0.,-1.)) ;
#2969 = DIRECTION('',(0.,0.,-1.)) ;
#2970 = DIRECTION('',(0.,-1.,0.)) ;
#2971 = DIRECTION('center_axis',(0.,1.,0.)) ;
#2972 = DIRECTION('ref_axis',(0.,0.,1.)) ;
#2973 = DIRECTION('',(0.,0.,-1.)) ;
#2974 = DIRECTION('',(1.,0.,0.)) ;
#2975 = DIRECTION('center_axis',(1.,0.,0.)) ;
#2976 = DIRECTION('ref_axis',(0.,0.,-1.)) ;
#2977 = DIRECTION('',(0.,0.,-1.)) ;
#2978 = DIRECTION('',(0.,-1.,0.)) ;
#2979 = DIRECTION('center_axis',(0.,0.,-1.)) ;
#2980 = DIRECTION('ref_axis',(-1.,0.,0.)) ;
#2981 = DIRECTION('center_axis',(0.,0.,-1.)) ;
#2982 = DIRECTION('ref_axis',(-1.,0.,0.)) ;
#2983 = DIRECTION('center_axis',(0.,0.,-1.)) ;
#2984 = DIRECTION('ref_axis',(-1.,0.,0.)) ;
#2985 = DIRECTION('axis',(0.,0.,1.)) ;
#2986 = DIRECTION('refdir',(1.,0.,0.)) ;
#2987 = DIRECTION('center_axis',(2.50028956146539E-17,2.89689231211468E-18,
1.)) ;
#2988 = DIRECTION('ref_axis',(1.,-8.74300631892311E-16,-2.50028956146539E-17)) ;
#2989 = DIRECTION('center_axis',(2.50028956146539E-17,2.89689231211468E-18,
1.)) ;
#2990 = DIRECTION('ref_axis',(-1.,8.74300631892311E-16,2.50028956146539E-17)) ;
#2991 = DIRECTION('',(2.50028956146539E-17,2.89689231211468E-18,1.)) ;
#2992 = DIRECTION('center_axis',(2.50028956146539E-17,2.89689231211468E-18,
1.)) ;
#2993 = DIRECTION('ref_axis',(-1.,8.74300631892311E-16,2.50028956146539E-17)) ;
#2994 = DIRECTION('',(2.50028956146539E-17,2.89689231211468E-18,1.)) ;
#2995 = DIRECTION('center_axis',(1.,-6.07748371951869E-14,-2.50028956146538E-17)) ;
#2996 = DIRECTION('ref_axis',(-6.07748371951869E-14,-1.,2.8968923121162E-18)) ;
#2997 = DIRECTION('',(6.07748371951869E-14,1.,-2.8968923121162E-18)) ;
#2998 = DIRECTION('',(2.50028956146539E-17,2.89689231211468E-18,1.)) ;
#2999 = DIRECTION('',(6.07748371951869E-14,1.,-2.8968923121162E-18)) ;
#3000 = DIRECTION('center_axis',(2.50028956146539E-17,2.89689231211468E-18,
1.)) ;
#3001 = DIRECTION('ref_axis',(1.,-8.74300631892311E-16,-2.50028956146539E-17)) ;
#3002 = DIRECTION('center_axis',(2.50028956146539E-17,2.89689231211468E-18,
1.)) ;
#3003 = DIRECTION('ref_axis',(1.,-8.74300631892311E-16,-2.50028956146539E-17)) ;
#3004 = DIRECTION('',(2.50028956146539E-17,2.89689231211468E-18,1.)) ;
#3005 = DIRECTION('center_axis',(2.50028956146539E-17,2.89689231211468E-18,
1.)) ;
#3006 = DIRECTION('ref_axis',(1.,-8.74300631892311E-16,-2.50028956146539E-17)) ;
#3007 = DIRECTION('center_axis',(9.96765311807047E-16,1.,-2.8968923121147E-18)) ;
#3008 = DIRECTION('ref_axis',(1.,-9.96765311807047E-16,-2.50028956146539E-17)) ;
#3009 = DIRECTION('',(-1.,9.96765311807047E-16,2.50028956146539E-17)) ;
#3010 = DIRECTION('',(-1.,9.96765311807047E-16,2.50028956146539E-17)) ;
#3011 = DIRECTION('center_axis',(-2.50028956146539E-17,-2.89689231211468E-18,
-1.)) ;
#3012 = DIRECTION('ref_axis',(-1.,8.74300631892311E-16,2.50028956146539E-17)) ;
#3013 = DIRECTION('center_axis',(-2.50028956146539E-17,-2.89689231211468E-18,
-1.)) ;
#3014 = DIRECTION('ref_axis',(-1.,8.74300631892311E-16,2.50028956146539E-17)) ;
#3015 = DIRECTION('',(0.,0.,1.)) ;
#3016 = DIRECTION('',(1.,0.,0.)) ;
#3017 = DIRECTION('',(0.,0.,1.)) ;
#3018 = DIRECTION('',(1.,0.,0.)) ;
#3019 = DIRECTION('',(0.,0.,1.)) ;
#3020 = DIRECTION('',(1.,0.,0.)) ;
#3021 = DIRECTION('',(0.,0.,1.)) ;
#3022 = DIRECTION('',(1.,0.,0.)) ;
#3023 = DIRECTION('',(0.,0.,1.)) ;
#3024 = DIRECTION('',(1.,0.,0.)) ;
#3025 = DIRECTION('',(0.,0.,1.)) ;
#3026 = DIRECTION('',(1.,0.,0.)) ;
#3027 = DIRECTION('',(0.,0.,1.)) ;
#3028 = DIRECTION('',(1.,0.,0.)) ;
#3029 = DIRECTION('',(0.,0.,1.)) ;
#3030 = DIRECTION('',(1.,0.,0.)) ;
#3031 = CARTESIAN_POINT('',(0.,0.,0.)) ;
#3032 = CARTESIAN_POINT('',(0.,0.,0.)) ;
#3033 = CARTESIAN_POINT('Origin',(0.,0.,-4.8)) ;
#3034 = CARTESIAN_POINT('',(-47.5,-5.81707229594993E-15,-4.8)) ;
#3035 = CARTESIAN_POINT('Origin',(0.,0.,-4.8)) ;
#3036 = CARTESIAN_POINT('',(-47.5,-5.81707229594993E-15,0.)) ;
#3037 = CARTESIAN_POINT('',(-47.5,-5.81707229594993E-15,-4.8)) ;
#3038 = CARTESIAN_POINT('Origin',(0.,0.,0.)) ;
#3039 = CARTESIAN_POINT('Origin',(0.,465.,-4.8)) ;
#3040 = CARTESIAN_POINT('',(305.5,465.,0.)) ;
#3041 = CARTESIAN_POINT('',(-225.,465.,0.)) ;
#3042 = CARTESIAN_POINT('',(0.,465.,0.)) ;
#3043 = CARTESIAN_POINT('',(305.5,465.,-4.8)) ;
#3044 = CARTESIAN_POINT('',(305.5,465.,-4.8)) ;
#3045 = CARTESIAN_POINT('',(-225.,465.,-4.8)) ;
#3046 = CARTESIAN_POINT('',(-225.,465.,-4.8)) ;
#3047 = CARTESIAN_POINT('',(-225.,465.,-4.8)) ;
#3048 = CARTESIAN_POINT('Origin',(305.5,465.,-4.8)) ;
#3049 = CARTESIAN_POINT('',(305.5,550.,0.)) ;
#3050 = CARTESIAN_POINT('',(305.5,465.,0.)) ;
#3051 = CARTESIAN_POINT('',(305.5,550.,-4.8)) ;
#3052 = CARTESIAN_POINT('',(305.5,550.,-4.8)) ;
#3053 = CARTESIAN_POINT('',(305.5,465.,-4.8)) ;
#3054 = CARTESIAN_POINT('Origin',(305.5,550.,-4.8)) ;
#3055 = CARTESIAN_POINT('',(890.,550.,0.)) ;
#3056 = CARTESIAN_POINT('',(305.5,550.,0.)) ;
#3057 = CARTESIAN_POINT('',(890.,550.,-4.8)) ;
#3058 = CARTESIAN_POINT('',(890.,550.,-4.8)) ;
#3059 = CARTESIAN_POINT('',(305.5,550.,-4.8)) ;
#3060 = CARTESIAN_POINT('Origin',(890.,550.,-4.8)) ;
#3061 = CARTESIAN_POINT('',(890.,-1.0683737973463E-15,0.)) ;
#3062 = CARTESIAN_POINT('',(890.,550.,0.)) ;
#3063 = CARTESIAN_POINT('',(890.,-1.0683737973463E-15,-4.8)) ;
#3064 = CARTESIAN_POINT('',(890.,-1.0683737973463E-15,-4.8)) ;
#3065 = CARTESIAN_POINT('',(890.,550.,-4.8)) ;
#3066 = CARTESIAN_POINT('Origin',(100.,0.,-4.8)) ;
#3067 = CARTESIAN_POINT('',(-690.,1.35308431126191E-13,0.)) ;
#3068 = CARTESIAN_POINT('Origin',(100.,0.,0.)) ;
#3069 = CARTESIAN_POINT('',(-690.,1.35308431126191E-13,-4.8)) ;
#3070 = CARTESIAN_POINT('',(-690.,1.35308431126191E-13,-4.8)) ;
#3071 = CARTESIAN_POINT('Origin',(100.,1.35308431126191E-13,-4.8)) ;
#3072 = CARTESIAN_POINT('Origin',(-225.,1.35308431126191E-13,-4.8)) ;
#3073 = CARTESIAN_POINT('Origin',(-225.,1.35308431126191E-13,0.)) ;
#3074 = CARTESIAN_POINT('Origin',(-225.,1.35308431126191E-13,-4.8)) ;
#3075 = CARTESIAN_POINT('Origin',(100.,0.,-4.8)) ;
#3076 = CARTESIAN_POINT('Origin',(100.,0.,0.)) ;
#3077 = CARTESIAN_POINT('',(0.,0.,0.)) ;
#3078 = CARTESIAN_POINT('Origin',(-68.281612705649,343.274848141115,456.5)) ;
#3079 = CARTESIAN_POINT('',(-74.7816127056665,343.274848141115,456.5)) ;
#3080 = CARTESIAN_POINT('Origin',(-68.281612705649,343.274848141115,456.5)) ;
#3081 = CARTESIAN_POINT('',(-74.7816127056665,343.274848141115,461.3)) ;
#3082 = CARTESIAN_POINT('',(-74.7816127056665,343.274848141115,456.5)) ;
#3083 = CARTESIAN_POINT('Origin',(-68.281612705649,343.274848141115,461.3)) ;
#3084 = CARTESIAN_POINT('Origin',(-194.449581556862,291.014364305891,456.5)) ;
#3085 = CARTESIAN_POINT('',(-200.949581556867,291.014364305891,456.5)) ;
#3086 = CARTESIAN_POINT('Origin',(-194.449581556862,291.014364305891,456.5)) ;
#3087 = CARTESIAN_POINT('',(-200.949581556867,291.014364305891,461.3)) ;
#3088 = CARTESIAN_POINT('',(-200.949581556867,291.014364305891,456.5)) ;
#3089 = CARTESIAN_POINT('Origin',(-194.449581556862,291.014364305891,461.3)) ;
#3090 = CARTESIAN_POINT('Origin',(-291.014364305892,194.44958155686,456.5)) ;
#3091 = CARTESIAN_POINT('',(-297.514364305897,194.44958155686,456.5)) ;
#3092 = CARTESIAN_POINT('Origin',(-291.014364305892,194.44958155686,456.5)) ;
#3093 = CARTESIAN_POINT('',(-297.514364305897,194.44958155686,461.3)) ;
#3094 = CARTESIAN_POINT('',(-297.514364305896,194.44958155686,456.5)) ;
#3095 = CARTESIAN_POINT('Origin',(-291.014364305892,194.44958155686,461.3)) ;
#3096 = CARTESIAN_POINT('Origin',(-343.274848141133,68.2816127056437,456.5)) ;
#3097 = CARTESIAN_POINT('',(-349.774848141137,68.2816127056437,456.5)) ;
#3098 = CARTESIAN_POINT('Origin',(-343.274848141133,68.2816127056437,456.5)) ;
#3099 = CARTESIAN_POINT('',(-349.774848141137,68.2816127056437,461.3)) ;
#3100 = CARTESIAN_POINT('',(-349.774848141137,68.2816127056437,456.5)) ;
#3101 = CARTESIAN_POINT('Origin',(-343.274848141133,68.2816127056437,461.3)) ;
#3102 = CARTESIAN_POINT('Origin',(-343.274848141133,-68.2816127056468,456.5)) ;
#3103 = CARTESIAN_POINT('',(-349.774848141136,-68.2816127056468,456.5)) ;
#3104 = CARTESIAN_POINT('Origin',(-343.274848141133,-68.2816127056468,456.5)) ;
#3105 = CARTESIAN_POINT('',(-349.774848141136,-68.2816127056468,461.3)) ;
#3106 = CARTESIAN_POINT('',(-349.774848141137,-68.2816127056468,456.5)) ;
#3107 = CARTESIAN_POINT('Origin',(-343.274848141133,-68.2816127056468,461.3)) ;
#3108 = CARTESIAN_POINT('Origin',(-291.014364305893,-194.449581556863,456.5)) ;
#3109 = CARTESIAN_POINT('',(-297.514364305895,-194.449581556863,456.5)) ;
#3110 = CARTESIAN_POINT('Origin',(-291.014364305893,-194.449581556863,456.5)) ;
#3111 = CARTESIAN_POINT('',(-297.514364305895,-194.449581556863,461.3)) ;
#3112 = CARTESIAN_POINT('',(-297.514364305896,-194.449581556863,456.5)) ;
#3113 = CARTESIAN_POINT('Origin',(-291.014364305893,-194.449581556863,461.3)) ;
#3114 = CARTESIAN_POINT('Origin',(-194.449581556862,-291.014364305894,456.5)) ;
#3115 = CARTESIAN_POINT('',(-200.949581556864,-291.014364305894,456.5)) ;
#3116 = CARTESIAN_POINT('Origin',(-194.449581556862,-291.014364305894,456.5)) ;
#3117 = CARTESIAN_POINT('',(-200.949581556864,-291.014364305894,461.3)) ;
#3118 = CARTESIAN_POINT('',(-200.949581556864,-291.014364305894,456.5)) ;
#3119 = CARTESIAN_POINT('Origin',(-194.449581556862,-291.014364305894,461.3)) ;
#3120 = CARTESIAN_POINT('Origin',(-68.2816127056456,-343.274848141134,456.5)) ;
#3121 = CARTESIAN_POINT('',(-74.7816127056465,-343.274848141134,456.5)) ;
#3122 = CARTESIAN_POINT('Origin',(-68.2816127056456,-343.274848141134,456.5)) ;
#3123 = CARTESIAN_POINT('',(-74.7816127056465,-343.274848141134,461.3)) ;
#3124 = CARTESIAN_POINT('',(-74.7816127056465,-343.274848141134,456.5)) ;
#3125 = CARTESIAN_POINT('Origin',(-68.2816127056456,-343.274848141134,461.3)) ;
#3126 = CARTESIAN_POINT('Origin',(68.2816127056448,-343.274848141134,456.5)) ;
#3127 = CARTESIAN_POINT('',(61.7816127056446,-343.274848141134,456.5)) ;
#3128 = CARTESIAN_POINT('Origin',(68.2816127056448,-343.274848141134,456.5)) ;
#3129 = CARTESIAN_POINT('',(61.7816127056446,-343.274848141134,461.3)) ;
#3130 = CARTESIAN_POINT('',(61.7816127056446,-343.274848141134,456.5)) ;
#3131 = CARTESIAN_POINT('Origin',(68.2816127056448,-343.274848141134,461.3)) ;
#3132 = CARTESIAN_POINT('Origin',(194.449581556861,-291.014364305894,456.5)) ;
#3133 = CARTESIAN_POINT('',(187.949581556862,-291.014364305894,456.5)) ;
#3134 = CARTESIAN_POINT('Origin',(194.449581556861,-291.014364305894,456.5)) ;
#3135 = CARTESIAN_POINT('',(187.949581556862,-291.014364305894,461.3)) ;
#3136 = CARTESIAN_POINT('',(187.949581556862,-291.014364305894,456.5)) ;
#3137 = CARTESIAN_POINT('Origin',(194.449581556861,-291.014364305894,461.3)) ;
#3138 = CARTESIAN_POINT('Origin',(291.014364305892,-194.449581556863,456.5)) ;
#3139 = CARTESIAN_POINT('',(284.514364305893,-194.449581556863,456.5)) ;
#3140 = CARTESIAN_POINT('Origin',(291.014364305892,-194.449581556863,456.5)) ;
#3141 = CARTESIAN_POINT('',(284.514364305893,-194.449581556863,461.3)) ;
#3142 = CARTESIAN_POINT('',(284.514364305893,-194.449581556863,456.5)) ;
#3143 = CARTESIAN_POINT('Origin',(291.014364305892,-194.449581556863,461.3)) ;
#3144 = CARTESIAN_POINT('Origin',(343.274848141132,-68.2816127056467,456.5)) ;
#3145 = CARTESIAN_POINT('',(336.774848141133,-68.2816127056467,456.5)) ;
#3146 = CARTESIAN_POINT('Origin',(343.274848141132,-68.2816127056467,456.5)) ;
#3147 = CARTESIAN_POINT('',(336.774848141133,-68.2816127056467,461.3)) ;
#3148 = CARTESIAN_POINT('',(336.774848141133,-68.2816127056467,456.5)) ;
#3149 = CARTESIAN_POINT('Origin',(343.274848141132,-68.2816127056467,461.3)) ;
#3150 = CARTESIAN_POINT('Origin',(343.274848141132,68.2816127056437,456.5)) ;
#3151 = CARTESIAN_POINT('',(336.774848141133,68.2816127056437,456.5)) ;
#3152 = CARTESIAN_POINT('Origin',(343.274848141132,68.2816127056437,456.5)) ;
#3153 = CARTESIAN_POINT('',(336.774848141133,68.2816127056437,461.3)) ;
#3154 = CARTESIAN_POINT('',(336.774848141133,68.2816127056437,456.5)) ;
#3155 = CARTESIAN_POINT('Origin',(343.274848141132,68.2816127056437,461.3)) ;
#3156 = CARTESIAN_POINT('Origin',(291.014364305892,194.44958155686,456.5)) ;
#3157 = CARTESIAN_POINT('',(284.514364305893,194.44958155686,456.5)) ;
#3158 = CARTESIAN_POINT('Origin',(291.014364305892,194.44958155686,456.5)) ;
#3159 = CARTESIAN_POINT('',(284.514364305893,194.44958155686,461.3)) ;
#3160 = CARTESIAN_POINT('',(284.514364305893,194.44958155686,456.5)) ;
#3161 = CARTESIAN_POINT('Origin',(291.014364305892,194.44958155686,461.3)) ;
#3162 = CARTESIAN_POINT('Origin',(194.44958155687,291.014364305904,456.5)) ;
#3163 = CARTESIAN_POINT('',(187.949581556878,291.014364305904,456.5)) ;
#3164 = CARTESIAN_POINT('Origin',(194.44958155687,291.014364305904,456.5)) ;
#3165 = CARTESIAN_POINT('',(187.949581556878,291.014364305904,461.3)) ;
#3166 = CARTESIAN_POINT('',(187.949581556878,291.014364305904,456.5)) ;
#3167 = CARTESIAN_POINT('Origin',(194.44958155687,291.014364305904,461.3)) ;
#3168 = CARTESIAN_POINT('Origin',(68.2816127056448,343.274848141131,456.5)) ;
#3169 = CARTESIAN_POINT('',(61.7816127056448,343.274848141131,456.5)) ;
#3170 = CARTESIAN_POINT('Origin',(68.2816127056448,343.274848141131,456.5)) ;
#3171 = CARTESIAN_POINT('',(61.7816127056448,343.274848141131,461.3)) ;
#3172 = CARTESIAN_POINT('',(61.7816127056448,343.274848141131,456.5)) ;
#3173 = CARTESIAN_POINT('Origin',(68.2816127056448,343.274848141131,461.3)) ;
#3174 = CARTESIAN_POINT('Origin',(-1.79110198894605E-13,1.12074915713733E-13,
456.5)) ;
#3175 = CARTESIAN_POINT('',(-285.,7.71724819380337E-14,456.5)) ;
#3176 = CARTESIAN_POINT('Origin',(-1.79110198894605E-13,1.12074915713733E-13,
456.5)) ;
#3177 = CARTESIAN_POINT('',(-285.,7.71724819380337E-14,461.3)) ;
#3178 = CARTESIAN_POINT('',(-285.,7.71724819380334E-14,456.5)) ;
#3179 = CARTESIAN_POINT('Origin',(-1.79110198894605E-13,1.12074915713733E-13,
461.3)) ;
#3180 = CARTESIAN_POINT('Origin',(-1.23599047663348E-13,465.,456.5)) ;
#3181 = CARTESIAN_POINT('',(300.5,465.,461.3)) ;
#3182 = CARTESIAN_POINT('',(-225.,465.,461.3)) ;
#3183 = CARTESIAN_POINT('',(-1.23599047663348E-13,465.,461.3)) ;
#3184 = CARTESIAN_POINT('',(300.5,465.,456.5)) ;
#3185 = CARTESIAN_POINT('',(300.5,465.,456.5)) ;
#3186 = CARTESIAN_POINT('',(-225.,465.,456.5)) ;
#3187 = CARTESIAN_POINT('',(-225.,465.,456.5)) ;
#3188 = CARTESIAN_POINT('',(-225.,465.,456.5)) ;
#3189 = CARTESIAN_POINT('Origin',(300.5,465.,456.5)) ;
#3190 = CARTESIAN_POINT('',(300.5,550.,461.3)) ;
#3191 = CARTESIAN_POINT('',(300.5,465.,461.3)) ;
#3192 = CARTESIAN_POINT('',(300.5,550.,456.5)) ;
#3193 = CARTESIAN_POINT('',(300.5,550.,456.5)) ;
#3194 = CARTESIAN_POINT('',(300.5,465.,456.5)) ;
#3195 = CARTESIAN_POINT('Origin',(300.5,550.,456.5)) ;
#3196 = CARTESIAN_POINT('',(890.,550.,461.3)) ;
#3197 = CARTESIAN_POINT('',(300.5,550.,461.3)) ;
#3198 = CARTESIAN_POINT('',(890.,550.,456.5)) ;
#3199 = CARTESIAN_POINT('',(890.,550.,456.5)) ;
#3200 = CARTESIAN_POINT('',(300.5,550.,456.5)) ;
#3201 = CARTESIAN_POINT('Origin',(890.,550.,456.5)) ;
#3202 = CARTESIAN_POINT('',(890.,2.23097218176249E-13,461.3)) ;
#3203 = CARTESIAN_POINT('',(890.,550.,461.3)) ;
#3204 = CARTESIAN_POINT('',(890.,2.23097218176249E-13,456.5)) ;
#3205 = CARTESIAN_POINT('',(890.,2.23097218176249E-13,456.5)) ;
#3206 = CARTESIAN_POINT('',(890.,550.,456.5)) ;
#3207 = CARTESIAN_POINT('Origin',(99.9999999999998,1.12074915713733E-13,456.5)) ;
#3208 = CARTESIAN_POINT('',(-690.,1.12074915713733E-13,461.3)) ;
#3209 = CARTESIAN_POINT('Origin',(99.9999999999998,1.12074915713733E-13,461.3)) ;
#3210 = CARTESIAN_POINT('',(-690.,1.12074915713733E-13,456.5)) ;
#3211 = CARTESIAN_POINT('',(-690.,1.12074915713733E-13,456.5)) ;
#3212 = CARTESIAN_POINT('Origin',(99.9999999999998,1.12074915713733E-13,456.5)) ;
#3213 = CARTESIAN_POINT('Origin',(-225.,1.12074915713733E-13,456.5)) ;
#3214 = CARTESIAN_POINT('Origin',(-225.,1.12074915713733E-13,461.3)) ;
#3215 = CARTESIAN_POINT('Origin',(-225.,1.12074915713733E-13,456.5)) ;
#3216 = CARTESIAN_POINT('Origin',(99.9999999999998,1.12074915713733E-13,456.5)) ;
#3217 = CARTESIAN_POINT('Origin',(99.9999999999998,1.12074915713733E-13,461.3)) ;
#3218 = CARTESIAN_POINT('',(0.,0.,0.)) ;
#3219 = CARTESIAN_POINT('Origin',(300.2,560.,18.2500000000001)) ;
#3220 = CARTESIAN_POINT('',(300.2,560.,23.7500000000001)) ;
#3221 = CARTESIAN_POINT('Origin',(300.2,560.,18.2500000000001)) ;
#3222 = CARTESIAN_POINT('',(300.2,550.,23.7500000000001)) ;
#3223 = CARTESIAN_POINT('',(300.2,560.,23.7500000000001)) ;
#3224 = CARTESIAN_POINT('Origin',(300.2,550.,18.2500000000001)) ;
#3225 = CARTESIAN_POINT('Origin',(300.199999999999,560.,123.25)) ;
#3226 = CARTESIAN_POINT('',(300.199999999999,560.,128.75)) ;
#3227 = CARTESIAN_POINT('Origin',(300.199999999999,560.,123.25)) ;
#3228 = CARTESIAN_POINT('',(300.199999999999,550.,128.75)) ;
#3229 = CARTESIAN_POINT('',(300.199999999999,560.,128.75)) ;
#3230 = CARTESIAN_POINT('Origin',(300.199999999999,550.,123.25)) ;
#3231 = CARTESIAN_POINT('Origin',(300.199999999998,560.,228.25)) ;
#3232 = CARTESIAN_POINT('',(300.199999999998,560.,233.75)) ;
#3233 = CARTESIAN_POINT('Origin',(300.199999999998,560.,228.25)) ;
#3234 = CARTESIAN_POINT('',(300.199999999998,550.,233.75)) ;
#3235 = CARTESIAN_POINT('',(300.199999999998,560.,233.75)) ;
#3236 = CARTESIAN_POINT('Origin',(300.199999999998,550.,228.25)) ;
#3237 = CARTESIAN_POINT('Origin',(300.199999999997,560.,333.25)) ;
#3238 = CARTESIAN_POINT('',(300.199999999997,560.,338.75)) ;
#3239 = CARTESIAN_POINT('Origin',(300.199999999997,560.,333.25)) ;
#3240 = CARTESIAN_POINT('',(300.199999999997,550.,338.75)) ;
#3241 = CARTESIAN_POINT('',(300.199999999997,560.,338.75)) ;
#3242 = CARTESIAN_POINT('Origin',(300.199999999997,550.,333.25)) ;
#3243 = CARTESIAN_POINT('Origin',(300.199999999996,560.,438.25)) ;
#3244 = CARTESIAN_POINT('',(300.199999999996,560.,443.75)) ;
#3245 = CARTESIAN_POINT('Origin',(300.199999999996,560.,438.25)) ;
#3246 = CARTESIAN_POINT('',(300.199999999996,550.,443.75)) ;
#3247 = CARTESIAN_POINT('',(300.199999999996,560.,443.75)) ;
#3248 = CARTESIAN_POINT('Origin',(300.199999999996,550.,438.25)) ;
#3249 = CARTESIAN_POINT('Origin',(900.200000000004,560.,438.25)) ;
#3250 = CARTESIAN_POINT('',(900.200000000004,560.,443.75)) ;
#3251 = CARTESIAN_POINT('Origin',(900.200000000004,560.,438.25)) ;
#3252 = CARTESIAN_POINT('',(900.200000000004,550.,443.75)) ;
#3253 = CARTESIAN_POINT('',(900.200000000004,560.,443.75)) ;
#3254 = CARTESIAN_POINT('Origin',(900.200000000004,550.,438.25)) ;
#3255 = CARTESIAN_POINT('Origin',(900.200000000003,560.,333.25)) ;
#3256 = CARTESIAN_POINT('',(900.200000000003,560.,338.75)) ;
#3257 = CARTESIAN_POINT('Origin',(900.200000000003,560.,333.25)) ;
#3258 = CARTESIAN_POINT('',(900.200000000003,550.,338.75)) ;
#3259 = CARTESIAN_POINT('',(900.200000000003,560.,338.75)) ;
#3260 = CARTESIAN_POINT('Origin',(900.200000000003,550.,333.25)) ;
#3261 = CARTESIAN_POINT('Origin',(900.200000000002,560.,228.25)) ;
#3262 = CARTESIAN_POINT('',(900.200000000002,560.,233.75)) ;
#3263 = CARTESIAN_POINT('Origin',(900.200000000002,560.,228.25)) ;
#3264 = CARTESIAN_POINT('',(900.200000000002,550.,233.75)) ;
#3265 = CARTESIAN_POINT('',(900.200000000002,560.,233.75)) ;
#3266 = CARTESIAN_POINT('Origin',(900.200000000002,550.,228.25)) ;
#3267 = CARTESIAN_POINT('Origin',(900.200000000001,560.,123.25)) ;
#3268 = CARTESIAN_POINT('',(900.200000000001,560.,128.75)) ;
#3269 = CARTESIAN_POINT('Origin',(900.200000000001,560.,123.25)) ;
#3270 = CARTESIAN_POINT('',(900.200000000001,550.,128.75)) ;
#3271 = CARTESIAN_POINT('',(900.200000000001,560.,128.75)) ;
#3272 = CARTESIAN_POINT('Origin',(900.200000000001,550.,123.25)) ;
#3273 = CARTESIAN_POINT('Origin',(900.2,560.,18.2499999999999)) ;
#3274 = CARTESIAN_POINT('',(900.2,560.,23.75)) ;
#3275 = CARTESIAN_POINT('Origin',(900.2,560.,18.2499999999999)) ;
#3276 = CARTESIAN_POINT('',(900.2,550.,23.75)) ;
#3277 = CARTESIAN_POINT('',(900.2,560.,23.7499999999999)) ;
#3278 = CARTESIAN_POINT('Origin',(900.2,550.,18.2499999999999)) ;
#3279 = CARTESIAN_POINT('Origin',(350.2,560.,-16.7500000000003)) ;
#3280 = CARTESIAN_POINT('',(350.2,560.,-11.2500000000003)) ;
#3281 = CARTESIAN_POINT('Origin',(350.2,560.,-16.7500000000003)) ;
#3282 = CARTESIAN_POINT('',(350.2,550.,-11.2500000000003)) ;
#3283 = CARTESIAN_POINT('',(350.2,560.,-11.2500000000003)) ;
#3284 = CARTESIAN_POINT('Origin',(350.2,550.,-16.7500000000003)) ;
#3285 = CARTESIAN_POINT('Origin',(450.2,560.,-16.7500000000003)) ;
#3286 = CARTESIAN_POINT('',(450.2,560.,-11.2500000000003)) ;
#3287 = CARTESIAN_POINT('Origin',(450.2,560.,-16.7500000000003)) ;
#3288 = CARTESIAN_POINT('',(450.2,550.,-11.2500000000003)) ;
#3289 = CARTESIAN_POINT('',(450.2,560.,-11.2500000000003)) ;
#3290 = CARTESIAN_POINT('Origin',(450.2,550.,-16.7500000000003)) ;
#3291 = CARTESIAN_POINT('Origin',(550.2,560.,-16.7500000000003)) ;
#3292 = CARTESIAN_POINT('',(550.2,560.,-11.2500000000003)) ;
#3293 = CARTESIAN_POINT('Origin',(550.2,560.,-16.7500000000003)) ;
#3294 = CARTESIAN_POINT('',(550.2,550.,-11.2500000000003)) ;
#3295 = CARTESIAN_POINT('',(550.2,560.,-11.2500000000003)) ;
#3296 = CARTESIAN_POINT('Origin',(550.2,550.,-16.7500000000003)) ;
#3297 = CARTESIAN_POINT('Origin',(650.2,560.,-16.7500000000003)) ;
#3298 = CARTESIAN_POINT('',(650.2,560.,-11.2500000000003)) ;
#3299 = CARTESIAN_POINT('Origin',(650.2,560.,-16.7500000000003)) ;
#3300 = CARTESIAN_POINT('',(650.2,550.,-11.2500000000003)) ;
#3301 = CARTESIAN_POINT('',(650.2,560.,-11.2500000000003)) ;
#3302 = CARTESIAN_POINT('Origin',(650.2,550.,-16.7500000000003)) ;
#3303 = CARTESIAN_POINT('Origin',(750.2,560.,-16.7500000000003)) ;
#3304 = CARTESIAN_POINT('',(750.2,560.,-11.2500000000003)) ;
#3305 = CARTESIAN_POINT('Origin',(750.2,560.,-16.7500000000003)) ;
#3306 = CARTESIAN_POINT('',(750.2,550.,-11.2500000000003)) ;
#3307 = CARTESIAN_POINT('',(750.2,560.,-11.2500000000003)) ;
#3308 = CARTESIAN_POINT('Origin',(750.2,550.,-16.7500000000003)) ;
#3309 = CARTESIAN_POINT('Origin',(850.2,560.,-16.7500000000003)) ;
#3310 = CARTESIAN_POINT('',(850.2,560.,-11.2500000000003)) ;
#3311 = CARTESIAN_POINT('Origin',(850.2,560.,-16.7500000000003)) ;
#3312 = CARTESIAN_POINT('',(850.2,550.,-11.2500000000003)) ;
#3313 = CARTESIAN_POINT('',(850.2,560.,-11.2500000000003)) ;
#3314 = CARTESIAN_POINT('Origin',(850.2,550.,-16.7500000000003)) ;
#3315 = CARTESIAN_POINT('Origin',(850.2,560.,473.25)) ;
#3316 = CARTESIAN_POINT('',(850.2,560.,478.75)) ;
#3317 = CARTESIAN_POINT('Origin',(850.2,560.,473.25)) ;
#3318 = CARTESIAN_POINT('',(850.2,550.,478.75)) ;
#3319 = CARTESIAN_POINT('',(850.2,560.,478.75)) ;
#3320 = CARTESIAN_POINT('Origin',(850.2,550.,473.25)) ;
#3321 = CARTESIAN_POINT('Origin',(750.2,560.,473.25)) ;
#3322 = CARTESIAN_POINT('',(750.2,560.,478.75)) ;
#3323 = CARTESIAN_POINT('Origin',(750.2,560.,473.25)) ;
#3324 = CARTESIAN_POINT('',(750.2,550.,478.75)) ;
#3325 = CARTESIAN_POINT('',(750.2,560.,478.75)) ;
#3326 = CARTESIAN_POINT('Origin',(750.2,550.,473.25)) ;
#3327 = CARTESIAN_POINT('Origin',(650.2,560.,473.25)) ;
#3328 = CARTESIAN_POINT('',(650.2,560.,478.75)) ;
#3329 = CARTESIAN_POINT('Origin',(650.2,560.,473.25)) ;
#3330 = CARTESIAN_POINT('',(650.2,550.,478.75)) ;
#3331 = CARTESIAN_POINT('',(650.2,560.,478.75)) ;
#3332 = CARTESIAN_POINT('Origin',(650.2,550.,473.25)) ;
#3333 = CARTESIAN_POINT('Origin',(550.2,560.,473.25)) ;
#3334 = CARTESIAN_POINT('',(550.2,560.,478.75)) ;
#3335 = CARTESIAN_POINT('Origin',(550.2,560.,473.25)) ;
#3336 = CARTESIAN_POINT('',(550.2,550.,478.75)) ;
#3337 = CARTESIAN_POINT('',(550.2,560.,478.75)) ;
#3338 = CARTESIAN_POINT('Origin',(550.2,550.,473.25)) ;
#3339 = CARTESIAN_POINT('Origin',(450.2,560.,473.25)) ;
#3340 = CARTESIAN_POINT('',(450.2,560.,478.75)) ;
#3341 = CARTESIAN_POINT('Origin',(450.2,560.,473.25)) ;
#3342 = CARTESIAN_POINT('',(450.2,550.,478.75)) ;
#3343 = CARTESIAN_POINT('',(450.2,560.,478.75)) ;
#3344 = CARTESIAN_POINT('Origin',(450.2,550.,473.25)) ;
#3345 = CARTESIAN_POINT('Origin',(350.2,560.,473.25)) ;
#3346 = CARTESIAN_POINT('',(350.2,560.,478.75)) ;
#3347 = CARTESIAN_POINT('Origin',(350.2,560.,473.25)) ;
#3348 = CARTESIAN_POINT('',(350.2,550.,478.75)) ;
#3349 = CARTESIAN_POINT('',(350.2,560.,478.75)) ;
#3350 = CARTESIAN_POINT('Origin',(350.2,550.,473.25)) ;
#3351 = CARTESIAN_POINT('Origin',(600.2,560.,228.25)) ;
#3352 = CARTESIAN_POINT('',(280.2,560.,-26.75)) ;
#3353 = CARTESIAN_POINT('',(280.2,560.,483.25)) ;
#3354 = CARTESIAN_POINT('',(280.2,560.,-26.75)) ;
#3355 = CARTESIAN_POINT('',(290.2,560.,493.25)) ;
#3356 = CARTESIAN_POINT('',(280.2,560.,483.25)) ;
#3357 = CARTESIAN_POINT('',(910.2,560.,493.25)) ;
#3358 = CARTESIAN_POINT('',(290.2,560.,493.25)) ;
#3359 = CARTESIAN_POINT('',(920.2,560.,483.25)) ;
#3360 = CARTESIAN_POINT('',(910.2,560.,493.25)) ;
#3361 = CARTESIAN_POINT('',(920.2,560.,-26.7500000000001)) ;
#3362 = CARTESIAN_POINT('',(920.2,560.,-26.7500000000001)) ;
#3363 = CARTESIAN_POINT('',(910.2,560.,-36.7500000000001)) ;
#3364 = CARTESIAN_POINT('',(910.2,560.,-36.7500000000001)) ;
#3365 = CARTESIAN_POINT('',(290.2,560.,-36.7500000000001)) ;
#3366 = CARTESIAN_POINT('',(290.2,560.,-36.7500000000001)) ;
#3367 = CARTESIAN_POINT('',(290.2,560.,-36.7500000000001)) ;
#3368 = CARTESIAN_POINT('',(880.2,560.,3.24999999999995)) ;
#3369 = CARTESIAN_POINT('',(320.2,560.,3.24999999999995)) ;
#3370 = CARTESIAN_POINT('',(320.2,560.,3.24999999999995)) ;
#3371 = CARTESIAN_POINT('',(880.2,560.,453.25)) ;
#3372 = CARTESIAN_POINT('',(880.2,560.,3.24999999999995)) ;
#3373 = CARTESIAN_POINT('',(320.2,560.,453.25)) ;
#3374 = CARTESIAN_POINT('',(320.2,560.,453.25)) ;
#3375 = CARTESIAN_POINT('',(320.2,560.,3.24999999999995)) ;
#3376 = CARTESIAN_POINT('Origin',(600.2,550.,228.25)) ;
#3377 = CARTESIAN_POINT('',(280.2,550.,-26.75)) ;
#3378 = CARTESIAN_POINT('',(280.2,550.,483.25)) ;
#3379 = CARTESIAN_POINT('',(280.2,550.,-26.75)) ;
#3380 = CARTESIAN_POINT('',(290.2,550.,-36.7500000000001)) ;
#3381 = CARTESIAN_POINT('',(290.2,550.,-36.7500000000001)) ;
#3382 = CARTESIAN_POINT('',(910.2,550.,-36.7500000000001)) ;
#3383 = CARTESIAN_POINT('',(290.2,550.,-36.7500000000001)) ;
#3384 = CARTESIAN_POINT('',(920.2,550.,-26.7500000000001)) ;
#3385 = CARTESIAN_POINT('',(910.2,550.,-36.7500000000001)) ;
#3386 = CARTESIAN_POINT('',(920.2,550.,483.25)) ;
#3387 = CARTESIAN_POINT('',(920.2,550.,-26.7500000000001)) ;
#3388 = CARTESIAN_POINT('',(910.2,550.,493.25)) ;
#3389 = CARTESIAN_POINT('',(910.2,550.,493.25)) ;
#3390 = CARTESIAN_POINT('',(290.2,550.,493.25)) ;
#3391 = CARTESIAN_POINT('',(290.2,550.,493.25)) ;
#3392 = CARTESIAN_POINT('',(280.2,550.,483.25)) ;
#3393 = CARTESIAN_POINT('',(880.2,550.,453.25)) ;
#3394 = CARTESIAN_POINT('',(880.2,550.,3.24999999999995)) ;
#3395 = CARTESIAN_POINT('',(880.2,550.,3.24999999999995)) ;
#3396 = CARTESIAN_POINT('',(320.2,550.,3.24999999999995)) ;
#3397 = CARTESIAN_POINT('',(320.2,550.,3.24999999999995)) ;
#3398 = CARTESIAN_POINT('',(320.2,550.,453.25)) ;
#3399 = CARTESIAN_POINT('',(320.2,550.,3.24999999999995)) ;
#3400 = CARTESIAN_POINT('',(320.2,550.,453.25)) ;
#3401 = CARTESIAN_POINT('Origin',(280.2,560.,-26.75)) ;
#3402 = CARTESIAN_POINT('',(280.2,560.,483.25)) ;
#3403 = CARTESIAN_POINT('',(280.2,560.,-26.75)) ;
#3404 = CARTESIAN_POINT('Origin',(280.2,560.,483.25)) ;
#3405 = CARTESIAN_POINT('',(290.2,560.,493.25)) ;
#3406 = CARTESIAN_POINT('Origin',(290.2,560.,493.25)) ;
#3407 = CARTESIAN_POINT('',(910.2,560.,493.25)) ;
#3408 = CARTESIAN_POINT('Origin',(910.2,560.,493.25)) ;
#3409 = CARTESIAN_POINT('',(920.2,560.,483.25)) ;
#3410 = CARTESIAN_POINT('Origin',(920.2,560.,-26.7500000000001)) ;
#3411 = CARTESIAN_POINT('',(920.2,560.,-26.7500000000001)) ;
#3412 = CARTESIAN_POINT('Origin',(910.2,560.,-36.7500000000001)) ;
#3413 = CARTESIAN_POINT('',(910.2,560.,-36.7500000000001)) ;
#3414 = CARTESIAN_POINT('Origin',(290.2,560.,-36.7500000000001)) ;
#3415 = CARTESIAN_POINT('',(290.2,560.,-36.7500000000001)) ;
#3416 = CARTESIAN_POINT('Origin',(290.2,560.,-36.7500000000001)) ;
#3417 = CARTESIAN_POINT('Origin',(880.2,560.,3.24999999999995)) ;
#3418 = CARTESIAN_POINT('',(880.2,560.,453.25)) ;
#3419 = CARTESIAN_POINT('',(880.2,560.,3.24999999999995)) ;
#3420 = CARTESIAN_POINT('Origin',(320.2,560.,3.24999999999995)) ;
#3421 = CARTESIAN_POINT('',(320.2,560.,3.24999999999995)) ;
#3422 = CARTESIAN_POINT('Origin',(320.2,560.,3.24999999999995)) ;
#3423 = CARTESIAN_POINT('',(320.2,560.,453.25)) ;
#3424 = CARTESIAN_POINT('Origin',(320.2,560.,453.25)) ;
#3425 = CARTESIAN_POINT('',(0.,0.,0.)) ;
#3426 = CARTESIAN_POINT('Origin',(99.9999999999999,1.35813926733553E-13,456.5)) ;
#3427 = CARTESIAN_POINT('',(880.2,2.3136087000303E-13,-5.55111512312578E-14)) ;
#3428 = CARTESIAN_POINT('',(99.9999999999997,-780.2,-5.55111512312578E-14)) ;
#3429 = CARTESIAN_POINT('Origin',(99.9999999999999,1.35813926733553E-13,-5.55111512312578E-14)) ;
#3430 = CARTESIAN_POINT('',(99.9999999999997,-780.2,456.5)) ;
#3431 = CARTESIAN_POINT('',(99.9999999999997,-780.2,456.5)) ;
#3432 = CARTESIAN_POINT('',(880.2,2.3136087000303E-13,456.5)) ;
#3433 = CARTESIAN_POINT('Origin',(99.9999999999999,1.35813926733553E-13,456.5)) ;
#3434 = CARTESIAN_POINT('',(880.2,2.3136087000303E-13,456.5)) ;
#3435 = CARTESIAN_POINT('Origin',(100.,-785.,456.5)) ;
#3436 = CARTESIAN_POINT('',(100.,-785.,-5.55111512312578E-14)) ;
#3437 = CARTESIAN_POINT('',(100.,-785.,-5.55111512312578E-14)) ;
#3438 = CARTESIAN_POINT('',(100.,-785.,456.5)) ;
#3439 = CARTESIAN_POINT('',(100.,-785.,456.5)) ;
#3440 = CARTESIAN_POINT('',(100.,-785.,456.5)) ;
#3441 = CARTESIAN_POINT('Origin',(99.9999999999999,1.35813926733553E-13,456.5)) ;
#3442 = CARTESIAN_POINT('',(885.,2.3194870046662E-13,-5.55111512312578E-14)) ;
#3443 = CARTESIAN_POINT('Origin',(99.9999999999999,1.35813926733553E-13,-5.55111512312578E-14)) ;
#3444 = CARTESIAN_POINT('',(885.,2.3194870046662E-13,456.5)) ;
#3445 = CARTESIAN_POINT('',(885.,2.3194870046662E-13,456.5)) ;
#3446 = CARTESIAN_POINT('Origin',(99.9999999999999,1.35813926733553E-13,456.5)) ;
#3447 = CARTESIAN_POINT('Origin',(880.2,2.3136087000303E-13,456.5)) ;
#3448 = CARTESIAN_POINT('',(880.2,2.3136087000303E-13,-5.55111512312578E-14)) ;
#3449 = CARTESIAN_POINT('',(880.2,2.3136087000303E-13,456.5)) ;
#3450 = CARTESIAN_POINT('Origin',(99.9999999999999,1.35813926733553E-13,456.5)) ;
#3451 = CARTESIAN_POINT('Origin',(99.9999999999999,1.35813926733553E-13,-5.55111512312578E-14)) ;
#3452 = CARTESIAN_POINT('',(0.,0.,0.)) ;
#3453 = CARTESIAN_POINT('Origin',(-23.3492724770243,413.445261297617,456.5)) ;
#3454 = CARTESIAN_POINT('',(-23.3492724770243,413.445261297617,-5.55111512312578E-14)) ;
#3455 = CARTESIAN_POINT('',(-25.453453981612,409.131049875381,-5.55111512312578E-14)) ;
#3456 = CARTESIAN_POINT('',(-23.3492724770243,413.445261297617,-5.55111512312578E-14)) ;
#3457 = CARTESIAN_POINT('',(-23.3492724770243,413.445261297617,456.5)) ;
#3458 = CARTESIAN_POINT('',(-23.3492724770243,413.445261297617,456.5)) ;
#3459 = CARTESIAN_POINT('',(-25.453453981612,409.131049875381,456.5)) ;
#3460 = CARTESIAN_POINT('',(-23.3492724770243,413.445261297617,456.5)) ;
#3461 = CARTESIAN_POINT('',(-25.453453981612,409.131049875381,456.5)) ;
#3462 = CARTESIAN_POINT('Origin',(-225.,2.51053816426691E-13,456.5)) ;
#3463 = CARTESIAN_POINT('',(-685.,2.51053816426691E-13,-5.55111512312578E-14)) ;
#3464 = CARTESIAN_POINT('Origin',(-225.,2.51053816426691E-13,-5.55111512312578E-14)) ;
#3465 = CARTESIAN_POINT('',(-685.,2.51053816426691E-13,456.5)) ;
#3466 = CARTESIAN_POINT('',(-685.,2.51053816426691E-13,456.5)) ;
#3467 = CARTESIAN_POINT('Origin',(-225.,2.51053816426691E-13,456.5)) ;
#3468 = CARTESIAN_POINT('Origin',(-680.200000000001,3.06799738723879E-13,
456.5)) ;
#3469 = CARTESIAN_POINT('',(-680.200000000001,3.06799738723879E-13,-5.55111512312578E-14)) ;
#3470 = CARTESIAN_POINT('',(-680.200000000001,3.06799738723879E-13,-5.55111512312578E-14)) ;
#3471 = CARTESIAN_POINT('',(-680.200000000001,3.06799738723879E-13,456.5)) ;
#3472 = CARTESIAN_POINT('',(-680.200000000001,3.06799738723879E-13,456.5)) ;
#3473 = CARTESIAN_POINT('',(-680.200000000001,3.06799738723879E-13,456.5)) ;
#3474 = CARTESIAN_POINT('Origin',(-225.,2.51053816426691E-13,456.5)) ;
#3475 = CARTESIAN_POINT('Origin',(-225.,2.51053816426691E-13,-5.55111512312578E-14)) ;
#3476 = CARTESIAN_POINT('Origin',(-225.,2.51053816426691E-13,456.5)) ;
#3477 = CARTESIAN_POINT('Origin',(-225.,2.51053816426691E-13,456.5)) ;
#3478 = CARTESIAN_POINT('Origin',(-225.,2.51053816426691E-13,-5.55111512312578E-14)) ;
#3479 = CARTESIAN_POINT('',(0.,0.,0.)) ;
#3480 = CARTESIAN_POINT('Origin',(884.999999999999,550.,456.5)) ;
#3481 = CARTESIAN_POINT('',(880.239999999999,5.55111512312578E-14,456.5)) ;
#3482 = CARTESIAN_POINT('',(880.239999999999,550.,456.5)) ;
#3483 = CARTESIAN_POINT('',(880.239999999999,550.,456.5)) ;
#3484 = CARTESIAN_POINT('',(884.999999999999,5.55111512312578E-14,456.5)) ;
#3485 = CARTESIAN_POINT('',(884.999999999999,5.55111512312578E-14,456.5)) ;
#3486 = CARTESIAN_POINT('',(884.999999999999,550.,456.5)) ;
#3487 = CARTESIAN_POINT('',(884.999999999999,550.,456.5)) ;
#3488 = CARTESIAN_POINT('',(884.999999999999,550.,456.5)) ;
#3489 = CARTESIAN_POINT('Origin',(884.999999999999,5.55111512312578E-14,5.55111512312578E-14)) ;
#3490 = CARTESIAN_POINT('',(880.239999999999,5.55111512312578E-14,5.55111512312578E-14)) ;
#3491 = CARTESIAN_POINT('',(880.239999999999,5.55111512312578E-14,5.55111512312578E-14)) ;
#3492 = CARTESIAN_POINT('',(884.999999999999,5.55111512312578E-14,5.55111512312578E-14)) ;
#3493 = CARTESIAN_POINT('',(884.999999999999,5.55111512312578E-14,5.55111512312578E-14)) ;
#3494 = CARTESIAN_POINT('',(884.999999999999,5.55111512312578E-14,5.55111512312578E-14)) ;
#3495 = CARTESIAN_POINT('Origin',(884.999999999999,550.,-5.55111512312578E-14)) ;
#3496 = CARTESIAN_POINT('',(880.239999999999,550.,-5.55111512312578E-14)) ;
#3497 = CARTESIAN_POINT('',(880.239999999999,550.,-5.55111512312578E-14)) ;
#3498 = CARTESIAN_POINT('',(884.999999999999,550.,-5.55111512312578E-14)) ;
#3499 = CARTESIAN_POINT('',(884.999999999999,550.,-5.55111512312578E-14)) ;
#3500 = CARTESIAN_POINT('',(884.999999999999,550.,-5.55111512312578E-14)) ;
#3501 = CARTESIAN_POINT('Origin',(884.999999999999,550.,-5.55111512312578E-14)) ;
#3502 = CARTESIAN_POINT('',(880.239999999999,550.,-5.55111512312578E-14)) ;
#3503 = CARTESIAN_POINT('',(884.999999999999,550.,-5.55111512312578E-14)) ;
#3504 = CARTESIAN_POINT('Origin',(884.999999999999,275.,228.25)) ;
#3505 = CARTESIAN_POINT('Origin',(880.239999999999,275.,228.25)) ;
#3506 = CARTESIAN_POINT('',(0.,0.,0.)) ;
#3507 = CARTESIAN_POINT('Origin',(294.2,409.,456.5)) ;
#3508 = CARTESIAN_POINT('',(294.2,409.,456.5)) ;
#3509 = CARTESIAN_POINT('',(294.2,413.8,456.5)) ;
#3510 = CARTESIAN_POINT('',(294.2,409.,456.5)) ;
#3511 = CARTESIAN_POINT('',(320.2,435.000000000001,456.5)) ;
#3512 = CARTESIAN_POINT('Origin',(294.2,435.,456.5)) ;
#3513 = CARTESIAN_POINT('',(315.4,435.,456.5)) ;
#3514 = CARTESIAN_POINT('',(315.4,435.,456.5)) ;
#3515 = CARTESIAN_POINT('Origin',(294.2,435.,456.5)) ;
#3516 = CARTESIAN_POINT('Origin',(315.4,435.,456.5)) ;
#3517 = CARTESIAN_POINT('',(-23.4000000000002,409.,456.5)) ;
#3518 = CARTESIAN_POINT('',(294.2,409.,456.5)) ;
#3519 = CARTESIAN_POINT('',(-23.4000000000002,413.8,456.5)) ;
#3520 = CARTESIAN_POINT('',(294.2,413.8,456.5)) ;
#3521 = CARTESIAN_POINT('',(-23.4000000000002,409.,456.5)) ;
#3522 = CARTESIAN_POINT('Origin',(320.2,435.000000000001,-5.55111512312578E-14)) ;
#3523 = CARTESIAN_POINT('',(320.2,435.000000000001,-5.55111512312578E-14)) ;
#3524 = CARTESIAN_POINT('',(315.4,435.,-5.55111512312578E-14)) ;
#3525 = CARTESIAN_POINT('',(320.2,435.000000000001,-5.55111512312578E-14)) ;
#3526 = CARTESIAN_POINT('',(294.2,409.,-5.55111512312578E-14)) ;
#3527 = CARTESIAN_POINT('Origin',(294.2,435.,-5.55111512312578E-14)) ;
#3528 = CARTESIAN_POINT('',(294.2,413.8,-5.55111512312578E-14)) ;
#3529 = CARTESIAN_POINT('',(294.2,413.8,-5.55111512312578E-14)) ;
#3530 = CARTESIAN_POINT('Origin',(294.2,435.,-5.55111512312578E-14)) ;
#3531 = CARTESIAN_POINT('Origin',(294.2,413.8,-5.55111512312578E-14)) ;
#3532 = CARTESIAN_POINT('',(320.2,550.,-5.55111512312578E-14)) ;
#3533 = CARTESIAN_POINT('',(320.2,550.,-5.55111512312578E-14)) ;
#3534 = CARTESIAN_POINT('',(315.4,550.,-5.55111512312578E-14)) ;
#3535 = CARTESIAN_POINT('',(315.4,550.,-5.55111512312578E-14)) ;
#3536 = CARTESIAN_POINT('',(315.4,550.,-5.55111512312578E-14)) ;
#3537 = CARTESIAN_POINT('Origin',(294.2,413.8,456.5)) ;
#3538 = CARTESIAN_POINT('',(-23.4000000000002,413.8,-5.55111512312578E-14)) ;
#3539 = CARTESIAN_POINT('',(294.2,413.8,-5.55111512312578E-14)) ;
#3540 = CARTESIAN_POINT('',(-23.4000000000002,413.8,456.5)) ;
#3541 = CARTESIAN_POINT('',(294.2,413.8,456.5)) ;
#3542 = CARTESIAN_POINT('Origin',(-23.4000000000002,409.,456.5)) ;
#3543 = CARTESIAN_POINT('',(-23.4000000000002,409.,-5.55111512312578E-14)) ;
#3544 = CARTESIAN_POINT('',(-23.4000000000002,409.,-5.55111512312578E-14)) ;
#3545 = CARTESIAN_POINT('',(-23.4000000000002,409.,456.5)) ;
#3546 = CARTESIAN_POINT('Origin',(294.2,409.,456.5)) ;
#3547 = CARTESIAN_POINT('',(294.2,409.,-5.55111512312578E-14)) ;
#3548 = CARTESIAN_POINT('',(294.2,409.,456.5)) ;
#3549 = CARTESIAN_POINT('Origin',(294.2,435.,456.5)) ;
#3550 = CARTESIAN_POINT('',(320.2,435.000000000001,456.5)) ;
#3551 = CARTESIAN_POINT('Origin',(320.2,550.,456.5)) ;
#3552 = CARTESIAN_POINT('',(320.2,550.,456.5)) ;
#3553 = CARTESIAN_POINT('',(320.2,550.,456.5)) ;
#3554 = CARTESIAN_POINT('',(320.2,550.,456.5)) ;
#3555 = CARTESIAN_POINT('Origin',(315.4,550.,456.5)) ;
#3556 = CARTESIAN_POINT('',(315.4,550.,456.5)) ;
#3557 = CARTESIAN_POINT('',(315.4,550.,456.5)) ;
#3558 = CARTESIAN_POINT('',(315.4,550.,456.5)) ;
#3559 = CARTESIAN_POINT('Origin',(315.4,550.,456.5)) ;
#3560 = CARTESIAN_POINT('',(315.4,435.,456.5)) ;
#3561 = CARTESIAN_POINT('',(315.4,550.,456.5)) ;
#3562 = CARTESIAN_POINT('Origin',(294.2,435.,456.5)) ;
#3563 = CARTESIAN_POINT('Origin',(294.2,435.,456.5)) ;
#3564 = CARTESIAN_POINT('Origin',(294.2,435.,-5.55111512312578E-14)) ;
#3565 = CARTESIAN_POINT('',(0.,0.,0.)) ;
#3566 = CARTESIAN_POINT('Origin',(99.9999999999999,1.35042597812193E-13,4.44089209850063E-13)) ;
#3567 = CARTESIAN_POINT('',(-680.2,9.14041325424531E-13,456.5)) ;
#3568 = CARTESIAN_POINT('',(99.9999999999994,-780.2,456.5)) ;
#3569 = CARTESIAN_POINT('Origin',(99.9999999999999,1.36365029152673E-13,456.5)) ;
#3570 = CARTESIAN_POINT('',(99.9999999999993,-780.2,4.44089209850063E-13)) ;
#3571 = CARTESIAN_POINT('',(99.9999999999993,-780.2,4.44089209850063E-13)) ;
#3572 = CARTESIAN_POINT('',(-680.2,9.1271889408405E-13,4.71844785465692E-13)) ;
#3573 = CARTESIAN_POINT('Origin',(99.9999999999999,1.35042597812193E-13,4.44089209850063E-13)) ;
#3574 = CARTESIAN_POINT('',(-680.2,9.1271889408405E-13,4.71844785465692E-13)) ;
#3575 = CARTESIAN_POINT('Origin',(99.999999999999,-785.,4.44089209850063E-13)) ;
#3576 = CARTESIAN_POINT('',(99.9999999999991,-785.,456.5)) ;
#3577 = CARTESIAN_POINT('',(99.9999999999991,-785.,456.5)) ;
#3578 = CARTESIAN_POINT('',(99.999999999999,-785.,4.44089209850063E-13)) ;
#3579 = CARTESIAN_POINT('',(99.999999999999,-785.,4.44089209850063E-13)) ;
#3580 = CARTESIAN_POINT('',(99.999999999999,-785.,4.44089209850063E-13)) ;
#3581 = CARTESIAN_POINT('Origin',(99.9999999999999,1.35042597812193E-13,4.44089209850063E-13)) ;
#3582 = CARTESIAN_POINT('',(-685.,9.18825798921204E-13,456.5)) ;
#3583 = CARTESIAN_POINT('Origin',(99.9999999999999,1.36365029152673E-13,456.5)) ;
#3584 = CARTESIAN_POINT('',(-685.,9.17503367580724E-13,4.71844785465692E-13)) ;
#3585 = CARTESIAN_POINT('',(-685.,9.17503367580724E-13,4.71844785465692E-13)) ;
#3586 = CARTESIAN_POINT('Origin',(99.9999999999999,1.35042597812193E-13,4.44089209850063E-13)) ;
#3587 = CARTESIAN_POINT('Origin',(-680.2,9.1271889408405E-13,4.71844785465692E-13)) ;
#3588 = CARTESIAN_POINT('',(-680.2,9.14041325424531E-13,456.5)) ;
#3589 = CARTESIAN_POINT('',(-680.2,9.1271889408405E-13,4.71844785465692E-13)) ;
#3590 = CARTESIAN_POINT('Origin',(99.9999999999999,1.35042597812193E-13,4.44089209850063E-13)) ;
#3591 = CARTESIAN_POINT('Origin',(99.9999999999999,1.36365029152673E-13,456.5)) ;
#3592 = CARTESIAN_POINT('',(0.,0.,0.)) ;
#3593 = CARTESIAN_POINT('',(0.,0.,0.)) ;
#3594 = CARTESIAN_POINT('',(0.,0.,0.)) ;
#3595 = CARTESIAN_POINT('',(0.,0.,0.)) ;
#3596 = CARTESIAN_POINT('',(0.,0.,0.)) ;
#3597 = CARTESIAN_POINT('',(0.,0.,0.)) ;
#3598 = CARTESIAN_POINT('',(0.,0.,0.)) ;
#3599 = CARTESIAN_POINT('',(0.,0.,0.)) ;
#3600 = UNCERTAINTY_MEASURE_WITH_UNIT(LENGTH_MEASURE(0.01),#3620,
'DISTANCE_ACCURACY_VALUE',
'Maximum model space distance between geometric entities at asserted c
onnectivities') ;
#3601 = UNCERTAINTY_MEASURE_WITH_UNIT(LENGTH_MEASURE(0.01),#3620,
'DISTANCE_ACCURACY_VALUE',
'Maximum model space distance between geometric entities at asserted c
onnectivities') ;
#3602 = UNCERTAINTY_MEASURE_WITH_UNIT(LENGTH_MEASURE(0.01),#3620,
'DISTANCE_ACCURACY_VALUE',
'Maximum model space distance between geometric entities at asserted c
onnectivities') ;
#3603 = UNCERTAINTY_MEASURE_WITH_UNIT(LENGTH_MEASURE(0.01),#3620,
'DISTANCE_ACCURACY_VALUE',
'Maximum model space distance between geometric entities at asserted c
onnectivities') ;
#3604 = UNCERTAINTY_MEASURE_WITH_UNIT(LENGTH_MEASURE(0.01),#3620,
'DISTANCE_ACCURACY_VALUE',
'Maximum model space distance between geometric entities at asserted c
onnectivities') ;
#3605 = UNCERTAINTY_MEASURE_WITH_UNIT(LENGTH_MEASURE(0.01),#3620,
'DISTANCE_ACCURACY_VALUE',
'Maximum model space distance between geometric entities at asserted c
onnectivities') ;
#3606 = UNCERTAINTY_MEASURE_WITH_UNIT(LENGTH_MEASURE(0.01),#3620,
'DISTANCE_ACCURACY_VALUE',
'Maximum model space distance between geometric entities at asserted c
onnectivities') ;
#3607 = UNCERTAINTY_MEASURE_WITH_UNIT(LENGTH_MEASURE(0.01),#3620,
'DISTANCE_ACCURACY_VALUE',
'Maximum model space distance between geometric entities at asserted c
onnectivities') ;
#3608 = UNCERTAINTY_MEASURE_WITH_UNIT(LENGTH_MEASURE(0.01),#3620,
'DISTANCE_ACCURACY_VALUE',
'Maximum model space distance between geometric entities at asserted c
onnectivities') ;
#3609 = UNCERTAINTY_MEASURE_WITH_UNIT(LENGTH_MEASURE(0.01),#3620,
'DISTANCE_ACCURACY_VALUE',
'Maximum model space distance between geometric entities at asserted c
onnectivities') ;
#3610 = (
GEOMETRIC_REPRESENTATION_CONTEXT(3)
GLOBAL_UNCERTAINTY_ASSIGNED_CONTEXT((#3600))
GLOBAL_UNIT_ASSIGNED_CONTEXT((#3620,#3622,#3623))
REPRESENTATION_CONTEXT('','3D')
) ;
#3611 = (
GEOMETRIC_REPRESENTATION_CONTEXT(3)
GLOBAL_UNCERTAINTY_ASSIGNED_CONTEXT((#3601))
GLOBAL_UNIT_ASSIGNED_CONTEXT((#3620,#3622,#3623))
REPRESENTATION_CONTEXT('','3D')
) ;
#3612 = (
GEOMETRIC_REPRESENTATION_CONTEXT(3)
GLOBAL_UNCERTAINTY_ASSIGNED_CONTEXT((#3602))
GLOBAL_UNIT_ASSIGNED_CONTEXT((#3620,#3622,#3623))
REPRESENTATION_CONTEXT('','3D')
) ;
#3613 = (
GEOMETRIC_REPRESENTATION_CONTEXT(3)
GLOBAL_UNCERTAINTY_ASSIGNED_CONTEXT((#3603))
GLOBAL_UNIT_ASSIGNED_CONTEXT((#3620,#3622,#3623))
REPRESENTATION_CONTEXT('','3D')
) ;
#3614 = (
GEOMETRIC_REPRESENTATION_CONTEXT(3)
GLOBAL_UNCERTAINTY_ASSIGNED_CONTEXT((#3604))
GLOBAL_UNIT_ASSIGNED_CONTEXT((#3620,#3622,#3623))
REPRESENTATION_CONTEXT('','3D')
) ;
#3615 = (
GEOMETRIC_REPRESENTATION_CONTEXT(3)
GLOBAL_UNCERTAINTY_ASSIGNED_CONTEXT((#3605))
GLOBAL_UNIT_ASSIGNED_CONTEXT((#3620,#3622,#3623))
REPRESENTATION_CONTEXT('','3D')
) ;
#3616 = (
GEOMETRIC_REPRESENTATION_CONTEXT(3)
GLOBAL_UNCERTAINTY_ASSIGNED_CONTEXT((#3606))
GLOBAL_UNIT_ASSIGNED_CONTEXT((#3620,#3622,#3623))
REPRESENTATION_CONTEXT('','3D')
) ;
#3617 = (
GEOMETRIC_REPRESENTATION_CONTEXT(3)
GLOBAL_UNCERTAINTY_ASSIGNED_CONTEXT((#3607))
GLOBAL_UNIT_ASSIGNED_CONTEXT((#3620,#3622,#3623))
REPRESENTATION_CONTEXT('','3D')
) ;
#3618 = (
GEOMETRIC_REPRESENTATION_CONTEXT(3)
GLOBAL_UNCERTAINTY_ASSIGNED_CONTEXT((#3608))
GLOBAL_UNIT_ASSIGNED_CONTEXT((#3620,#3622,#3623))
REPRESENTATION_CONTEXT('','3D')
) ;
#3619 = (
GEOMETRIC_REPRESENTATION_CONTEXT(3)
GLOBAL_UNCERTAINTY_ASSIGNED_CONTEXT((#3609))
GLOBAL_UNIT_ASSIGNED_CONTEXT((#3620,#3622,#3623))
REPRESENTATION_CONTEXT('','3D')
) ;
#3620 = (
LENGTH_UNIT()
NAMED_UNIT(*)
SI_UNIT(.MILLI.,.METRE.)
) ;
#3621 = (
LENGTH_UNIT()
NAMED_UNIT(*)
SI_UNIT($,.METRE.)
) ;
#3622 = (
NAMED_UNIT(*)
PLANE_ANGLE_UNIT()
SI_UNIT($,.RADIAN.)
) ;
#3623 = (
NAMED_UNIT(*)
SI_UNIT($,.STERADIAN.)
SOLID_ANGLE_UNIT()
) ;
#3624 = SHAPE_DEFINITION_REPRESENTATION(#3633,#3650) ;
#3625 = SHAPE_DEFINITION_REPRESENTATION(#3634,#3651) ;
#3626 = SHAPE_DEFINITION_REPRESENTATION(#3635,#3652) ;
#3627 = SHAPE_DEFINITION_REPRESENTATION(#3636,#3653) ;
#3628 = SHAPE_DEFINITION_REPRESENTATION(#3637,#3654) ;
#3629 = SHAPE_DEFINITION_REPRESENTATION(#3638,#3655) ;
#3630 = SHAPE_DEFINITION_REPRESENTATION(#3639,#3656) ;
#3631 = SHAPE_DEFINITION_REPRESENTATION(#3640,#3657) ;
#3632 = SHAPE_DEFINITION_REPRESENTATION(#3641,#3658) ;
#3633 = PRODUCT_DEFINITION_SHAPE('',$,#3660) ;
#3634 = PRODUCT_DEFINITION_SHAPE('',$,#3661) ;
#3635 = PRODUCT_DEFINITION_SHAPE('',$,#3662) ;
#3636 = PRODUCT_DEFINITION_SHAPE('',$,#3663) ;
#3637 = PRODUCT_DEFINITION_SHAPE('',$,#3664) ;
#3638 = PRODUCT_DEFINITION_SHAPE('',$,#3665) ;
#3639 = PRODUCT_DEFINITION_SHAPE('',$,#3666) ;
#3640 = PRODUCT_DEFINITION_SHAPE('',$,#3667) ;
#3641 = PRODUCT_DEFINITION_SHAPE('',$,#3668) ;
#3642 = PRODUCT_DEFINITION_SHAPE($,$,#35) ;
#3643 = PRODUCT_DEFINITION_SHAPE($,$,#36) ;
#3644 = PRODUCT_DEFINITION_SHAPE($,$,#37) ;
#3645 = PRODUCT_DEFINITION_SHAPE($,$,#38) ;
#3646 = PRODUCT_DEFINITION_SHAPE($,$,#39) ;
#3647 = PRODUCT_DEFINITION_SHAPE($,$,#40) ;
#3648 = PRODUCT_DEFINITION_SHAPE($,$,#41) ;
#3649 = PRODUCT_DEFINITION_SHAPE($,$,#42) ;
#3650 = SHAPE_REPRESENTATION('',(#2180,#2401,#2402,#2403,#2404,#2405,#2406,
#2407,#2408),#3610) ;
#3651 = SHAPE_REPRESENTATION('',(#2181),#3611) ;
#3652 = SHAPE_REPRESENTATION('',(#2197),#3612) ;
#3653 = SHAPE_REPRESENTATION('',(#2261),#3613) ;
#3654 = SHAPE_REPRESENTATION('',(#2342),#3614) ;
#3655 = SHAPE_REPRESENTATION('',(#2353),#3615) ;
#3656 = SHAPE_REPRESENTATION('',(#2364),#3616) ;
#3657 = SHAPE_REPRESENTATION('',(#2371),#3617) ;
#3658 = SHAPE_REPRESENTATION('',(#2390),#3618) ;
#3659 = PRODUCT_DEFINITION_CONTEXT('part definition',#3688,'design') ;
#3660 = PRODUCT_DEFINITION('MAS-644','MAS-644',#3669,#3659) ;
#3661 = PRODUCT_DEFINITION('Side_Panel_1','Side_Panel_1',#3670,#3659) ;
#3662 = PRODUCT_DEFINITION('Side_Panel_2','Side_Panel_2',#3671,#3659) ;
#3663 = PRODUCT_DEFINITION('Vent_Panel','Vent_Panel',#3672,#3659) ;
#3664 = PRODUCT_DEFINITION('Housing_Section_1','Housing_Section_1',#3673,
#3659) ;
#3665 = PRODUCT_DEFINITION('Housing_Section_2','Housing_Section_2',#3674,
#3659) ;
#3666 = PRODUCT_DEFINITION('Divider_Plate','Divider_Plate',#3675,#3659) ;
#3667 = PRODUCT_DEFINITION('Mounting_Block','Mounting_Block',#3676,#3659) ;
#3668 = PRODUCT_DEFINITION('Housing_Section_3','Housing_Section_3',#3677,
#3659) ;
#3669 = PRODUCT_DEFINITION_FORMATION('',$,#3690) ;
#3670 = PRODUCT_DEFINITION_FORMATION('',$,#3691) ;
#3671 = PRODUCT_DEFINITION_FORMATION('',$,#3692) ;
#3672 = PRODUCT_DEFINITION_FORMATION('',$,#3693) ;
#3673 = PRODUCT_DEFINITION_FORMATION('',$,#3694) ;
#3674 = PRODUCT_DEFINITION_FORMATION('',$,#3695) ;
#3675 = PRODUCT_DEFINITION_FORMATION('',$,#3696) ;
#3676 = PRODUCT_DEFINITION_FORMATION('',$,#3697) ;
#3677 = PRODUCT_DEFINITION_FORMATION('',$,#3698) ;
#3678 = PRODUCT_RELATED_PRODUCT_CATEGORY('MAS-644','MAS-644',(#3690)) ;
#3679 = PRODUCT_RELATED_PRODUCT_CATEGORY('Side_Panel_1','Side_Panel_1',(#3691)) ;
#3680 = PRODUCT_RELATED_PRODUCT_CATEGORY('Side_Panel_2','Side_Panel_2',(#3692)) ;
#3681 = PRODUCT_RELATED_PRODUCT_CATEGORY('Vent_Panel','Vent_Panel',(#3693)) ;
#3682 = PRODUCT_RELATED_PRODUCT_CATEGORY('Housing_Section_1',
'Housing_Section_1',(#3694)) ;
#3683 = PRODUCT_RELATED_PRODUCT_CATEGORY('Housing_Section_2',
'Housing_Section_2',(#3695)) ;
#3684 = PRODUCT_RELATED_PRODUCT_CATEGORY('Divider_Plate','Divider_Plate',
(#3696)) ;
#3685 = PRODUCT_RELATED_PRODUCT_CATEGORY('Mounting_Block',
'Mounting_Block',(#3697)) ;
#3686 = PRODUCT_RELATED_PRODUCT_CATEGORY('Housing_Section_3',
'Housing_Section_3',(#3698)) ;
#3687 = APPLICATION_PROTOCOL_DEFINITION('international standard',
'automotive_design',2009,#3688) ;
#3688 = APPLICATION_CONTEXT(
'Core Data for Automotive Mechanical Design Process') ;
#3689 = PRODUCT_CONTEXT('part definition',#3688,'mechanical') ;
#3690 = PRODUCT('MAS-644','MAS-644',$,(#3689)) ;
#3691 = PRODUCT('Side_Panel_1','Side_Panel_1',$,(#3689)) ;
#3692 = PRODUCT('Side_Panel_2','Side_Panel_2',$,(#3689)) ;
#3693 = PRODUCT('Vent_Panel','Vent_Panel',$,(#3689)) ;
#3694 = PRODUCT('Housing_Section_1','Housing_Section_1',$,(#3689)) ;
#3695 = PRODUCT('Housing_Section_2','Housing_Section_2',$,(#3689)) ;
#3696 = PRODUCT('Divider_Plate','Divider_Plate',$,(#3689)) ;
#3697 = PRODUCT('Mounting_Block','Mounting_Block',$,(#3689)) ;
#3698 = PRODUCT('Housing_Section_3','Housing_Section_3',$,(#3689)) ;
#3699 = PRESENTATION_STYLE_ASSIGNMENT((#3701)) ;
#3700 = PRESENTATION_STYLE_ASSIGNMENT((#3702)) ;
#3701 = SURFACE_STYLE_USAGE(.BOTH.,#3703) ;
#3702 = SURFACE_STYLE_USAGE(.BOTH.,#3704) ;
#3703 = SURFACE_SIDE_STYLE('',(#3705)) ;
#3704 = SURFACE_SIDE_STYLE('',(#3706)) ;
#3705 = SURFACE_STYLE_FILL_AREA(#3707) ;
#3706 = SURFACE_STYLE_FILL_AREA(#3708) ;
#3707 = FILL_AREA_STYLE('Steel - Satin',(#3709)) ;
#3708 = FILL_AREA_STYLE('Opaque(202,209,238)',(#3710)) ;
#3709 = FILL_AREA_STYLE_COLOUR('Steel - Satin',#3711) ;
#3710 = FILL_AREA_STYLE_COLOUR('Opaque(202,209,238)',#3712) ;
#3711 = COLOUR_RGB('Steel - Satin', 0.09019608, 0.27058824, 0.51372549) ;
#3712 = COLOUR_RGB('Opaque(202,209,238)', 0.09019608, 0.27058824, 0.51372549) ;
ENDSEC;
END-ISO-10303-21;
